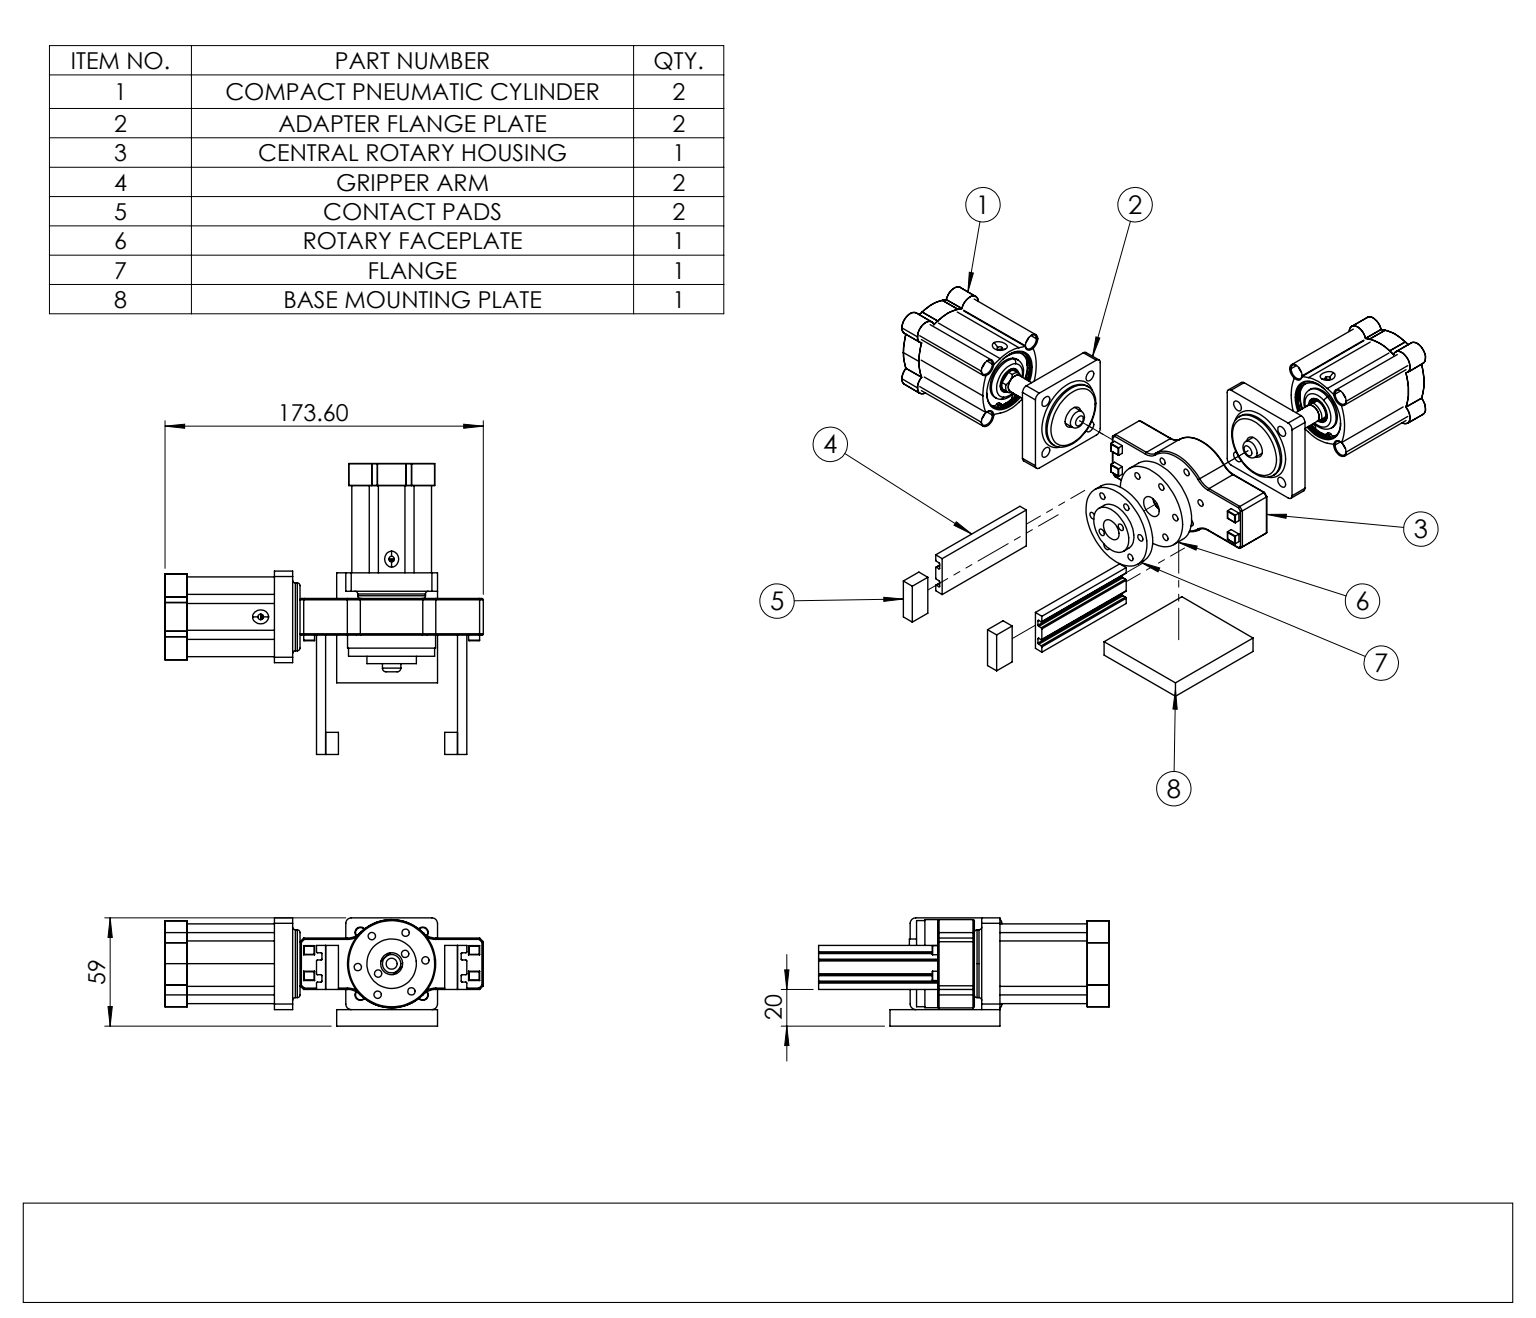
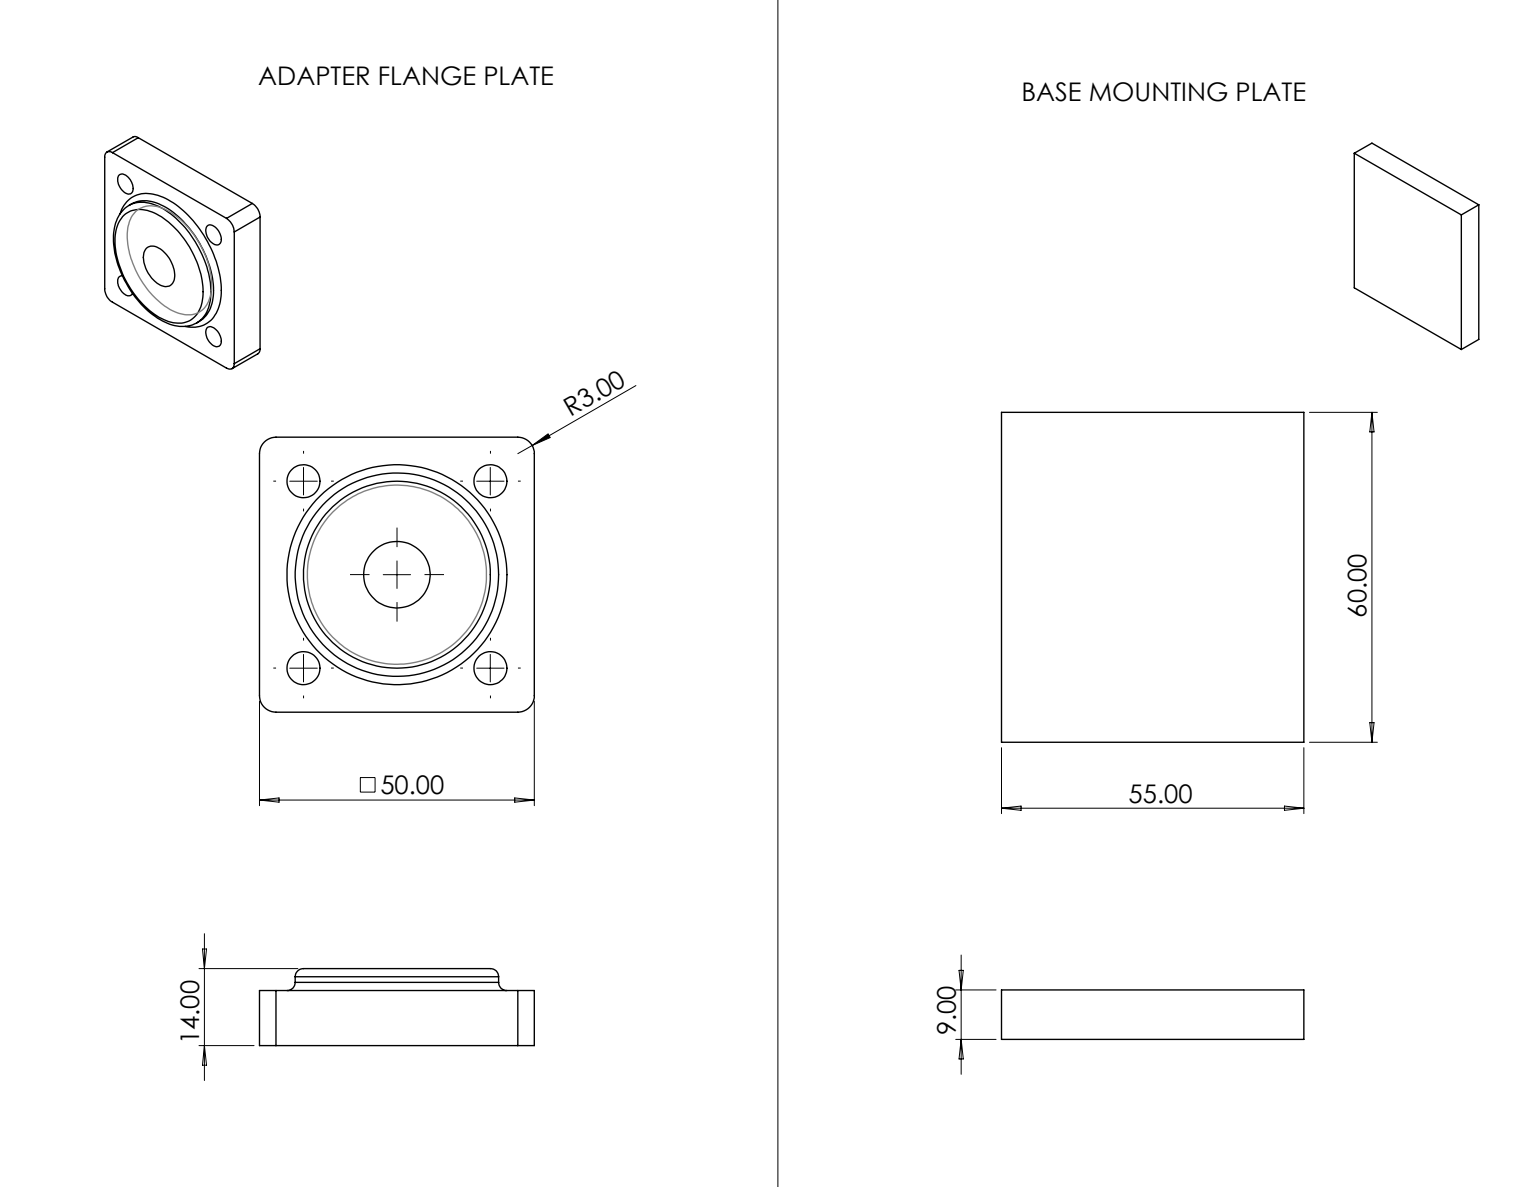
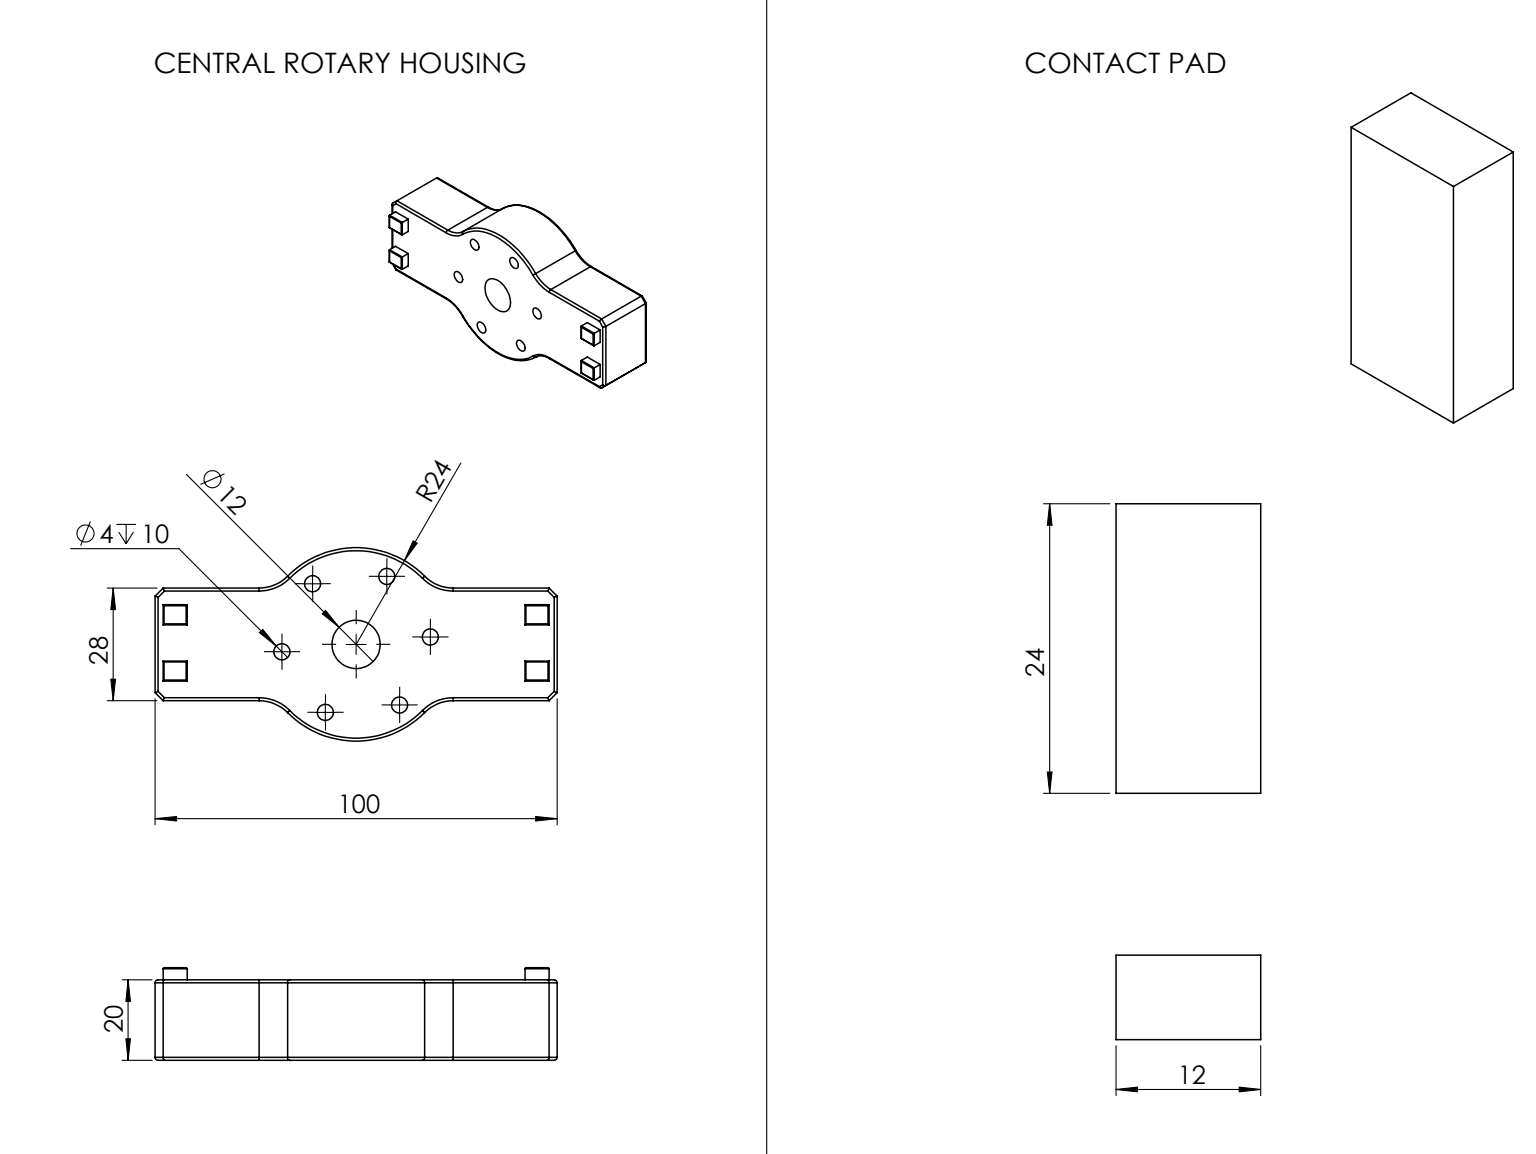
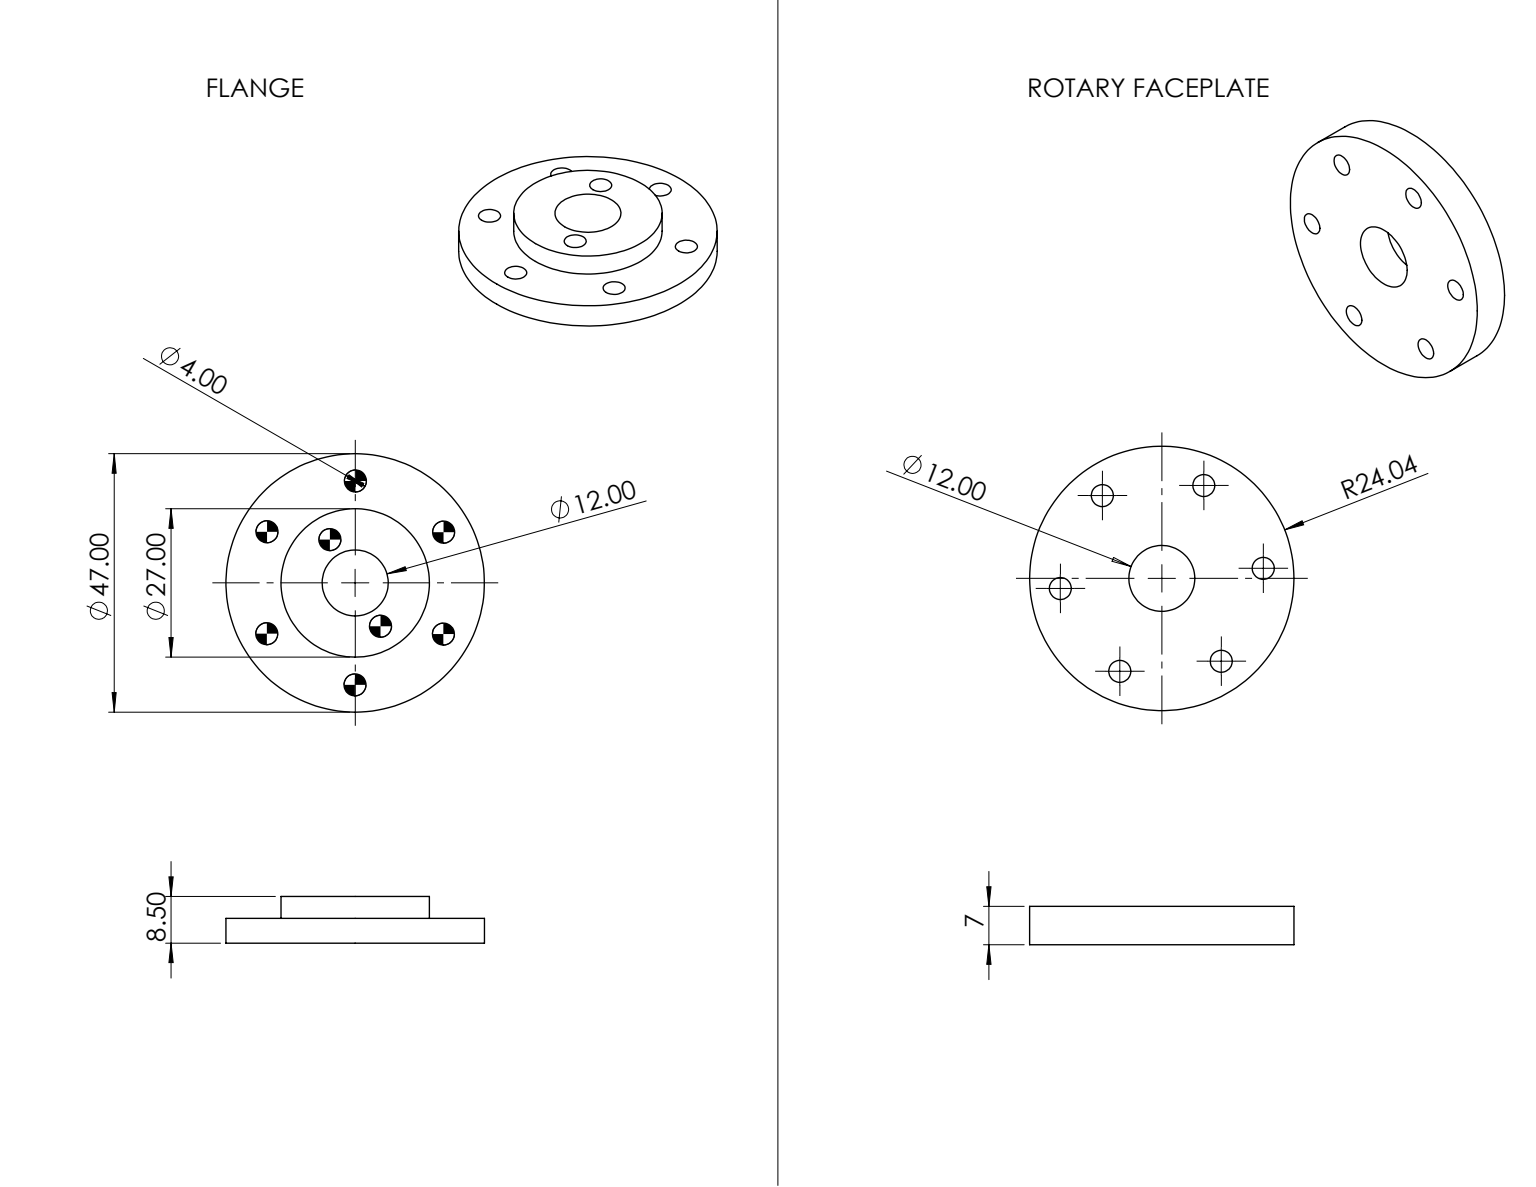
ISO-10303-21;
HEADER;
FILE_DESCRIPTION (('STEP AP214'),
    '1' );
FILE_NAME ('BR-Y-110',
    '2026-10-07T17:53:07',
    ( '' ),
    ( '' ),
    'SwSTEP 2.0',
    'SolidWorks 2025',
    '' );
FILE_SCHEMA (( 'AUTOMOTIVE_DESIGN' ));
ENDSEC;

DATA;
#1 = VERTEX_POINT ( 'NONE', #2797 ) ;
#2 = VERTEX_POINT ( 'NONE', #7279 ) ;
#3 = CARTESIAN_POINT ( 'NONE',  ( -18.05918829504999934, 10.97290950744599947, 5.250000000000000000 ) ) ;
#4 = FACE_OUTER_BOUND ( 'NONE', #8386, .T. ) ;
#5 = LINE ( 'NONE', #10836, #6273 ) ;
#6 = VERTEX_POINT ( 'NONE', #3958 ) ;
#7 = CARTESIAN_POINT ( 'NONE',  ( -0.04028432657539327000, 0.000000000000000000, 20.54539866546728533 ) ) ;
#8 = DIRECTION ( 'NONE',  ( -1.000000000000000000, 0.000000000000000000, 0.000000000000000000 ) ) ;
#9 = VECTOR ( 'NONE', #8104, 1000.000000000000000 ) ;
#10 = AXIS2_PLACEMENT_3D ( 'NONE', #13272, #6842, #503 ) ;
#11 = AXIS2_PLACEMENT_3D ( 'NONE', #8934, #9983, #13191 ) ;
#12 = CARTESIAN_POINT ( 'NONE',  ( -40.33164489498319938, 10.97290950744599947, 5.250000000000000000 ) ) ;
#13 = DIRECTION ( 'NONE',  ( 0.000000000000000000, 0.000000000000000000, 1.000000000000000000 ) ) ;
#14 = EDGE_CURVE ( 'NONE', #8213, #13437, #9334, .T. ) ;
#15 = ORIENTED_EDGE ( 'NONE', *, *, #6104, .F. ) ;
#16 = AXIS2_PLACEMENT_3D ( 'NONE', #5876, #10870, #7634 ) ;
#17 = DIRECTION ( 'NONE',  ( -1.000000000000000000, 0.000000000000000000, 0.000000000000000000 ) ) ;
#18 = VECTOR ( 'NONE', #2959, 1000.000000000000000 ) ;
#19 = CIRCLE ( 'NONE', #13399, 4.000000000000000888 ) ;
#20 = ORIENTED_EDGE ( 'NONE', *, *, #13229, .F. ) ;
#21 = ORIENTED_EDGE ( 'NONE', *, *, #12073, .F. ) ;
#22 = ORIENTED_EDGE ( 'NONE', *, *, #9153, .T. ) ;
#23 = EDGE_LOOP ( 'NONE', ( #6039, #6851, #1913, #2067 ) ) ;
#24 = CARTESIAN_POINT ( 'NONE',  ( -26.35918829505000005, 10.97290950744599947, 61.86500000000000199 ) ) ;
#25 = CARTESIAN_POINT ( 'NONE',  ( 43.38563590245419732, 87.34974178189119698, 20.00000000000000000 ) ) ;
#26 = EDGE_LOOP ( 'NONE', ( #8749, #11948, #13282, #3929 ) ) ;
#27 = DIRECTION ( 'NONE',  ( 0.000000000000000000, 0.000000000000000000, -1.000000000000000000 ) ) ;
#28 = FACE_OUTER_BOUND ( 'NONE', #13183, .T. ) ;
#29 = DIRECTION ( 'NONE',  ( 0.000000000000000000, -1.000000000000000000, 0.000000000000000000 ) ) ;
#30 = CARTESIAN_POINT ( 'NONE',  ( -18.05918829504999934, 10.97290950744599947, 57.35000000000000142 ) ) ;
#31 = DIRECTION ( 'NONE',  ( -0.000000000000000000, 1.000000000000000000, -0.000000000000000000 ) ) ;
#32 = VECTOR ( 'NONE', #959, 1000.000000000000000 ) ;
#33 = CIRCLE ( 'NONE', #3398, 4.749999999999997335 ) ;
#34 = ADVANCED_FACE ( 'NONE', ( #9475 ), #12553, .F. ) ;
#35 = ADVANCED_FACE ( 'NONE', ( #1932 ), #13451, .T. ) ;
#36 = EDGE_CURVE ( 'NONE', #826, #10489, #4183, .T. ) ;
#37 =( GEOMETRIC_REPRESENTATION_CONTEXT ( 3 ) GLOBAL_UNCERTAINTY_ASSIGNED_CONTEXT ( ( #1666 ) ) GLOBAL_UNIT_ASSIGNED_CONTEXT ( ( #5163, #1674, #7109 ) ) REPRESENTATION_CONTEXT ( 'NONE', 'WORKASPACE' ) );
#38 = CARTESIAN_POINT ( 'NONE',  ( 74.18094369249178044, 97.20665973629650125, 10.00000000000000000 ) ) ;
#39 = FACE_BOUND ( 'NONE', #10748, .T. ) ;
#40 = CARTESIAN_POINT ( 'NONE',  ( -23.49332020752115113, 0.2738342970428629952, 62.85000000000000142 ) ) ;
#41 = DIRECTION ( 'NONE',  ( 1.000000000000000000, 0.000000000000000000, 0.000000000000000000 ) ) ;
#42 = CARTESIAN_POINT ( 'NONE',  ( -18.32356812262639068, 30.35913048975403683, 52.99871736656052690 ) ) ;
#43 = DIRECTION ( 'NONE',  ( 0.000000000000000000, 1.000000000000000000, 0.000000000000000000 ) ) ;
#44 = CARTESIAN_POINT ( 'NONE',  ( -18.05918829505001355, 3.709013078446008027, 62.03182374100007479 ) ) ;
#45 = CARTESIAN_POINT ( 'NONE',  ( 68.49370948373500312, 113.0390816101113387, 0.7500000000000006661 ) ) ;
#46 = CARTESIAN_POINT ( 'NONE',  ( -1.904759825251885141, 5.678153534393399759, 62.14999999999999858 ) ) ;
#47 = DIRECTION ( 'NONE',  ( -0.000000000000000000, -0.000000000000000000, -1.000000000000000000 ) ) ;
#48 =( NAMED_UNIT ( * ) SI_UNIT ( $, .STERADIAN. ) SOLID_ANGLE_UNIT ( ) );
#49 = CONICAL_SURFACE ( 'NONE', #4748, 17.00000000000000000, 0.7853981633974476129 ) ;
#50 = EDGE_CURVE ( 'NONE', #1000, #13804, #2021, .T. ) ;
#51 = VERTEX_POINT ( 'NONE', #6255 ) ;
#52 = DIRECTION ( 'NONE',  ( 0.000000000000000000, 0.000000000000000000, 1.000000000000000000 ) ) ;
#53 = ORIENTED_EDGE ( 'NONE', *, *, #11858, .F. ) ;
#54 = VERTEX_POINT ( 'NONE', #10526 ) ;
#55 = CARTESIAN_POINT ( 'NONE',  ( -10.25088531517542023, -8.860076549334110041, 17.25000000000000000 ) ) ;
#56 = CIRCLE ( 'NONE', #12775, 5.000000000000000888 ) ;
#57 = CARTESIAN_POINT ( 'NONE',  ( -18.05918829504999934, 10.97290950744599947, 64.85000000000000853 ) ) ;
#58 = SURFACE_SIDE_STYLE ('',( #2323 ) ) ;
#59 = ORIENTED_EDGE ( 'NONE', *, *, #13776, .F. ) ;
#60 = PLANE ( 'NONE',  #2670 ) ;
#61 = EDGE_CURVE ( 'NONE', #8730, #12568, #7625, .T. ) ;
#62 = DIRECTION ( 'NONE',  ( 1.000000000000000000, 0.000000000000000000, 0.000000000000000000 ) ) ;
#63 = CARTESIAN_POINT ( 'NONE',  ( -5.631644894983189431, 10.97290950744599947, 17.25000000000000000 ) ) ;
#64 = AXIS2_PLACEMENT_3D ( 'NONE', #1240, #10758, #11538 ) ;
#65 = ORIENTED_EDGE ( 'NONE', *, *, #6040, .F. ) ;
#66 = EDGE_CURVE ( 'NONE', #2, #10148, #3731, .T. ) ;
#67 = CARTESIAN_POINT ( 'NONE',  ( 6.940811704950004213, 32.97290950744599769, 10.00000000000000000 ) ) ;
#68 = VERTEX_POINT ( 'NONE', #167 ) ;
#69 = FACE_OUTER_BOUND ( 'NONE', #8366, .T. ) ;
#70 = EDGE_CURVE ( 'NONE', #6919, #7844, #9610, .T. ) ;
#71 = DIRECTION ( 'NONE',  ( -1.000000000000000000, 0.000000000000000000, -0.000000000000000000 ) ) ;
#72 = CARTESIAN_POINT ( 'NONE',  ( 50.63563590245420443, 104.1554980190242361, 22.75000000000000000 ) ) ;
#73 = LINE ( 'NONE', #12845, #11581 ) ;
#74 = DIRECTION ( 'NONE',  ( 0.7071067811865451302, -0.7071067811865500152, 0.000000000000000000 ) ) ;
#75 = EDGE_CURVE ( 'NONE', #10483, #2779, #7556, .T. ) ;
#76 = AXIS2_PLACEMENT_3D ( 'NONE', #7169, #9139, #1729 ) ;
#77 = CARTESIAN_POINT ( 'NONE',  ( -24.37001676333060018, -4.028726038184999858, 62.14999999999999858 ) ) ;
#78 = FACE_OUTER_BOUND ( 'NONE', #2382, .T. ) ;
#79 = EDGE_LOOP ( 'NONE', ( #3659, #11191, #12245, #181 ) ) ;
#80 = EDGE_CURVE ( 'NONE', #9144, #4985, #2152, .T. ) ;
#81 = FACE_OUTER_BOUND ( 'NONE', #12463, .T. ) ;
#82 = ORIENTED_EDGE ( 'NONE', *, *, #9714, .T. ) ;
#83 = ORIENTED_EDGE ( 'NONE', *, *, #1868, .T. ) ;
#84 = EDGE_LOOP ( 'NONE', ( #6155, #12083, #10918, #3272 ) ) ;
#85 = DIRECTION ( 'NONE',  ( 0.000000000000000000, 0.000000000000000000, 1.000000000000000000 ) ) ;
#86 = DIRECTION ( 'NONE',  ( 0.7071067811865525687, 0.7071067811865425767, -0.000000000000000000 ) ) ;
#87 = VERTEX_POINT ( 'NONE', #8553 ) ;
#88 = EDGE_CURVE ( 'NONE', #10198, #10544, #1083, .T. ) ;
#89 = CARTESIAN_POINT ( 'NONE',  ( 142.6356359024541973, 87.03908161011133870, 19.25000000000000000 ) ) ;
#90 = CARTESIAN_POINT ( 'NONE',  ( -19.42965429280413048, 26.91526772932534683, 56.72114474750378577 ) ) ;
#91 = CARTESIAN_POINT ( 'NONE',  ( 7.347880794884120722E-16, 0.000000000000000000, -6.000000000000000888 ) ) ;
#92 = FACE_OUTER_BOUND ( 'NONE', #5027, .T. ) ;
#93 = DIRECTION ( 'NONE',  ( 0.000000000000000000, 0.000000000000000000, -1.000000000000000000 ) ) ;
#94 = ORIENTED_EDGE ( 'NONE', *, *, #9388, .F. ) ;
#95 = VERTEX_POINT ( 'NONE', #8619 ) ;
#96 = CARTESIAN_POINT ( 'NONE',  ( -15.05918829504999756, 10.97290950744599947, 118.8499999999999943 ) ) ;
#97 = ORIENTED_EDGE ( 'NONE', *, *, #11700, .F. ) ;
#98 = DIRECTION ( 'NONE',  ( 0.000000000000000000, 0.000000000000000000, 1.000000000000000000 ) ) ;
#99 = DIRECTION ( 'NONE',  ( 0.000000000000000000, 0.000000000000000000, 1.000000000000000000 ) ) ;
#100 = DIRECTION ( 'NONE',  ( 0.000000000000000000, 0.000000000000000000, -1.000000000000000000 ) ) ;
#101 = AXIS2_PLACEMENT_3D ( 'NONE', #2685, #3784, #6912 ) ;
#102 = CARTESIAN_POINT ( 'NONE',  ( 44.76431555889455183, 85.34974178189114014, 2.983588460272618114E-16 ) ) ;
#103 = CARTESIAN_POINT ( 'NONE',  ( -29.51816008892539855, -2.179141222803619993, 63.45000000000000284 ) ) ;
#104 = ORIENTED_EDGE ( 'NONE', *, *, #12811, .F. ) ;
#105 = CARTESIAN_POINT ( 'NONE',  ( -3.531395436049983960, 3.709013078445997369, 62.03182374100001084 ) ) ;
#106 = CARTESIAN_POINT ( 'NONE',  ( 141.8856359024541973, 87.34974178189115435, 20.00000000000000000 ) ) ;
#107 = CARTESIAN_POINT ( 'NONE',  ( -20.77625425128555392, 5.623371902244430842, 57.35000000000000142 ) ) ;
#108 = CARTESIAN_POINT ( 'NONE',  ( 123.1053058165644671, 129.5087515242213669, 0.7500000000000000000 ) ) ;
#109 =( LENGTH_UNIT ( ) NAMED_UNIT ( * ) SI_UNIT ( .MILLI., .METRE. ) );
#110 = CLOSED_SHELL ( 'NONE', ( #5060, #3881, #6623, #9987, #3732, #7105, #7461, #11688, #1191, #4265, #947, #3436, #2543, #10818, #12397, #3818, #11545, #6558, #4609, #2381, #2843, #3214, #13267, #5308, #5232, #10919, #9049, #5614, #7802, #750 ) ) ;
#111 = EDGE_CURVE ( 'NONE', #2836, #5819, #1718, .T. ) ;
#112 = EDGE_CURVE ( 'NONE', #4329, #209, #6197, .T. ) ;
#113 = AXIS2_PLACEMENT_3D ( 'NONE', #7430, #11720, #2167 ) ;
#114 = DIRECTION ( 'NONE',  ( 0.000000000000000000, 0.000000000000000000, 1.000000000000000000 ) ) ;
#115 = EDGE_LOOP ( 'NONE', ( #6121, #285 ) ) ;
#116 = ORIENTED_EDGE ( 'NONE', *, *, #8831, .F. ) ;
#117 = ORIENTED_EDGE ( 'NONE', *, *, #6877, .T. ) ;
#118 = PLANE ( 'NONE',  #6613 ) ;
#119 = DIRECTION ( 'NONE',  ( 0.000000000000000000, 0.000000000000000000, 1.000000000000000000 ) ) ;
#120 = CARTESIAN_POINT ( 'NONE',  ( 0.000000000000000000, 0.000000000000000000, 0.000000000000000000 ) ) ;
#121 = CYLINDRICAL_SURFACE ( 'NONE', #12455, 6.000000000000000888 ) ;
#122 = LINE ( 'NONE', #4468, #12298 ) ;
#123 = AXIS2_PLACEMENT_3D ( 'NONE', #1081, #954, #12877 ) ;
#124 = DIRECTION ( 'NONE',  ( 0.000000000000000000, 0.000000000000000000, 1.000000000000000000 ) ) ;
#125 = CARTESIAN_POINT ( 'NONE',  ( -18.05918829504999934, 10.97290950744599947, 68.84999999999999432 ) ) ;
#126 = EDGE_CURVE ( 'NONE', #1534, #5295, #6389, .T. ) ;
#127 = UNCERTAINTY_MEASURE_WITH_UNIT (LENGTH_MEASURE( 1.000000000000000082E-05 ), #7321, 'distance_accuracy_value', 'NONE');
#128 = ADVANCED_FACE ( 'NONE', ( #1149 ), #7351, .F. ) ;
#129 = VERTEX_POINT ( 'NONE', #4238 ) ;
#130 = EDGE_CURVE ( 'NONE', #6071, #11290, #13719, .T. ) ;
#131 = CARTESIAN_POINT ( 'NONE',  ( -15.41688231577083101, 30.20956267305470178, 54.20385837980890642 ) ) ;
#132 = SURFACE_STYLE_FILL_AREA ( #10766 ) ;
#133 = DIRECTION ( 'NONE',  ( 0.000000000000000000, 0.000000000000000000, 1.000000000000000000 ) ) ;
#134 = FACE_OUTER_BOUND ( 'NONE', #5191, .T. ) ;
#135 = VERTEX_POINT ( 'NONE', #8486 ) ;
#136 = PLANE ( 'NONE',  #5988 ) ;
#137 = DIRECTION ( 'NONE',  ( -0.000000000000000000, -0.000000000000000000, -1.000000000000000000 ) ) ;
#138 = DIRECTION ( 'NONE',  ( 0.000000000000000000, 0.000000000000000000, 1.000000000000000000 ) ) ;
#139 = ADVANCED_FACE ( 'NONE', ( #10588 ), #13367, .T. ) ;
#140 = VECTOR ( 'NONE', #5917, 1000.000000000000114 ) ;
#141 = DIRECTION ( 'NONE',  ( -0.000000000000000000, -0.000000000000000000, -1.000000000000000000 ) ) ;
#142 = ORIENTED_EDGE ( 'NONE', *, *, #754, .F. ) ;
#143 = EDGE_CURVE ( 'NONE', #7877, #9433, #12710, .T. ) ;
#144 = DIRECTION ( 'NONE',  ( 0.000000000000000000, 0.000000000000000000, -1.000000000000000000 ) ) ;
#145 = ORIENTED_EDGE ( 'NONE', *, *, #6603, .F. ) ;
#146 = ORIENTED_EDGE ( 'NONE', *, *, #5230, .T. ) ;
#147 = VECTOR ( 'NONE', #7020, 1000.000000000000000 ) ;
#148 = CARTESIAN_POINT ( 'NONE',  ( -25.33503448090910126, -7.245613863947209410, 64.85000000000000853 ) ) ;
#149 = LINE ( 'NONE', #12938, #855 ) ;
#150 = ORIENTED_EDGE ( 'NONE', *, *, #10812, .F. ) ;
#151 = CARTESIAN_POINT ( 'NONE',  ( -1.059188295049996231, -6.027090492554000534, 7.250000000000000000 ) ) ;
#152 = CARTESIAN_POINT ( 'NONE',  ( 5.999999999999999112, -12.00000000000000178, 7.000000000000000000 ) ) ;
#153 = LINE ( 'NONE', #1273, #6867 ) ;
#154 = CARTESIAN_POINT ( 'NONE',  ( -30.48673169511680214, 10.97290950744599947, 5.250000000000000000 ) ) ;
#155 = EDGE_CURVE ( 'NONE', #8675, #3193, #8240, .T. ) ;
#156 = FACE_OUTER_BOUND ( 'NONE', #2583, .T. ) ;
#157 = SHAPE_DEFINITION_REPRESENTATION ( #3699, #5502 ) ;
#158 = AXIS2_PLACEMENT_3D ( 'NONE', #4444, #13785, #5467 ) ;
#159 = VERTEX_POINT ( 'NONE', #3135 ) ;
#160 = VECTOR ( 'NONE', #1857, 1000.000000000000000 ) ;
#161 = EDGE_CURVE ( 'NONE', #11468, #4985, #9362, .T. ) ;
#162 = PRODUCT ( 'Contact Pads', 'Contact Pads', '', ( #11558 ) ) ;
#163 = EDGE_LOOP ( 'NONE', ( #919, #320, #6279, #11884 ) ) ;
#164 = EDGE_LOOP ( 'NONE', ( #8775, #9502, #10616, #5660 ) ) ;
#165 = FACE_OUTER_BOUND ( 'NONE', #7206, .T. ) ;
#166 = VECTOR ( 'NONE', #7008, 1000.000000000000000 ) ;
#167 = CARTESIAN_POINT ( 'NONE',  ( -32.05918829504999934, 27.97290950744599769, 10.00000000000000000 ) ) ;
#168 = CIRCLE ( 'NONE', #7293, 6.299999999999998046 ) ;
#169 = CARTESIAN_POINT ( 'NONE',  ( 3.500000000000001776, 2.000000000000000000, 0.000000000000000000 ) ) ;
#170 = AXIS2_PLACEMENT_3D ( 'NONE', #9398, #10575, #4153 ) ;
#171 = CARTESIAN_POINT ( 'NONE',  ( -20.25693731790400776, 30.25607652235614964, 53.78764270006948323 ) ) ;
#172 = VERTEX_POINT ( 'NONE', #11643 ) ;
#173 = CARTESIAN_POINT ( 'NONE',  ( -8.964285665223000521, 0.3335619008453594714, 62.14999999999999858 ) ) ;
#174 = DIRECTION ( 'NONE',  ( 1.000000000000000000, 0.000000000000000000, 0.000000000000000000 ) ) ;
#175 = CARTESIAN_POINT ( 'NONE',  ( -18.05918829504999934, 10.97290950744599947, 67.84999999999999432 ) ) ;
#176 = CARTESIAN_POINT ( 'NONE',  ( -18.05918829504999934, 10.97290950744599947, 56.84999999999999432 ) ) ;
#177 = VECTOR ( 'NONE', #8514, 1000.000000000000000 ) ;
#178 = AXIS2_PLACEMENT_3D ( 'NONE', #8254, #12725, #10295 ) ;
#179 = VECTOR ( 'NONE', #6554, 1000.000000000000000 ) ;
#180 = AXIS2_PLACEMENT_3D ( 'NONE', #7057, #3723, #3934 ) ;
#181 = ORIENTED_EDGE ( 'NONE', *, *, #4608, .T. ) ;
#182 = VERTEX_POINT ( 'NONE', #3404 ) ;
#183 = ORIENTED_EDGE ( 'NONE', *, *, #11008, .T. ) ;
#184 = DIRECTION ( 'NONE',  ( 0.000000000000000000, 0.000000000000000000, 1.000000000000000000 ) ) ;
#185 = ORIENTED_EDGE ( 'NONE', *, *, #5640, .F. ) ;
#186 = ADVANCED_FACE ( 'NONE', ( #7633, #11914, #39, #5265, #12757, #7419 ), #11708, .T. ) ;
#187 = EDGE_LOOP ( 'NONE', ( #9761, #8160, #4704, #9504 ) ) ;
#188 = DIRECTION ( 'NONE',  ( -0.000000000000000000, -0.000000000000000000, 1.000000000000000000 ) ) ;
#189 = VERTEX_POINT ( 'NONE', #4908 ) ;
#190 = FACE_OUTER_BOUND ( 'NONE', #11280, .T. ) ;
#191 = CARTESIAN_POINT ( 'NONE',  ( 0.000000000000000000, 0.000000000000000000, 7.000000000000000000 ) ) ;
#192 = VECTOR ( 'NONE', #12361, 1000.000000000000000 ) ;
#193 = FILL_AREA_STYLE_COLOUR ( '', #3402 ) ;
#194 = VERTEX_POINT ( 'NONE', #10221 ) ;
#195 = VECTOR ( 'NONE', #13133, 1000.000000000000114 ) ;
#196 = CARTESIAN_POINT ( 'NONE',  ( -35.05918829505000645, -6.027090492554000534, 7.250000000000000000 ) ) ;
#197 = DIRECTION ( 'NONE',  ( 0.000000000000000000, 0.000000000000000000, -1.000000000000000000 ) ) ;
#198 = VECTOR ( 'NONE', #6806, 999.9999999999998863 ) ;
#199 = CARTESIAN_POINT ( 'NONE',  ( -1.059188295049996231, 27.97290950744599769, 7.250000000000000000 ) ) ;
#200 = CARTESIAN_POINT ( 'NONE',  ( 62.16596598834396303, 68.56941169600129626, 20.00000000000000000 ) ) ;
#201 = ORIENTED_EDGE ( 'NONE', *, *, #8919, .T. ) ;
#202 = AXIS2_PLACEMENT_3D ( 'NONE', #3684, #7923, #11148 ) ;
#203 = CIRCLE ( 'NONE', #9813, 17.00000000000000355 ) ;
#204 = CARTESIAN_POINT ( 'NONE',  ( -16.07719306376069568, 30.27579076690150117, 53.62366803667482174 ) ) ;
#205 = ADVANCED_FACE ( 'NONE', ( #704 ), #2436, .F. ) ;
#206 = EDGE_CURVE ( 'NONE', #7753, #7831, #10944, .T. ) ;
#207 = ORIENTED_EDGE ( 'NONE', *, *, #1883, .F. ) ;
#208 = DIRECTION ( 'NONE',  ( 0.000000000000000000, 0.000000000000000000, 1.000000000000000000 ) ) ;
#209 = VERTEX_POINT ( 'NONE', #11330 ) ;
#210 = PRESENTATION_STYLE_ASSIGNMENT (( #5374 ) ) ;
#211 = CARTESIAN_POINT ( 'NONE',  ( 42.63563590245419732, 87.03908161011136713, 0.7500000000000006661 ) ) ;
#212 = FACE_OUTER_BOUND ( 'NONE', #7387, .T. ) ;
#213 = CARTESIAN_POINT ( 'NONE',  ( -24.10918829505000005, 10.97290950744599947, 64.85000000000000853 ) ) ;
#214 = AXIS2_PLACEMENT_3D ( 'NONE', #10840, #5509, #2126 ) ;
#215 = AXIS2_PLACEMENT_3D ( 'NONE', #11989, #2447, #13100 ) ;
#216 = ORIENTED_EDGE ( 'NONE', *, *, #2968, .F. ) ;
#217 = VERTEX_POINT ( 'NONE', #6667 ) ;
#218 = ORIENTED_EDGE ( 'NONE', *, *, #1514, .T. ) ;
#219 = DIRECTION ( 'NONE',  ( 0.000000000000000000, 0.000000000000000000, 1.000000000000000000 ) ) ;
#220 = ORIENTED_EDGE ( 'NONE', *, *, #13475, .F. ) ;
#221 = EDGE_CURVE ( 'NONE', #8225, #10962, #1891, .T. ) ;
#222 = ORIENTED_EDGE ( 'NONE', *, *, #6909, .F. ) ;
#223 = VERTEX_POINT ( 'NONE', #1688 ) ;
#224 = VECTOR ( 'NONE', #4940, 1000.000000000000114 ) ;
#225 = PRODUCT_DEFINITION_SHAPE ( 'NONE', 'NONE',  #13814 ) ;
#226 = CIRCLE ( 'NONE', #12506, 15.45000000000000462 ) ;
#227 = CONICAL_SURFACE ( 'NONE', #2931, 8.300000000000000711, 0.08573846772804097349 ) ;
#228 = AXIS2_PLACEMENT_3D ( 'NONE', #13430, #6224, #8258 ) ;
#230 = EDGE_CURVE ( 'NONE', #7248, #13568, #2901, .T. ) ;
#229 = MANIFOLD_SOLID_BREP ( 'Boss-Extrude1', #6124 ) ;
#231 = CYLINDRICAL_SURFACE ( 'NONE', #5745, 0.2500000000000002220 ) ;
#232 = DIRECTION ( 'NONE',  ( 0.000000000000000000, 0.000000000000000000, 1.000000000000000000 ) ) ;
#233 = EDGE_LOOP ( 'NONE', ( #8305, #2316, #6219, #5928, #5645 ) ) ;
#234 = EDGE_CURVE ( 'NONE', #8205, #12910, #5618, .T. ) ;
#235 = FACE_OUTER_BOUND ( 'NONE', #11663, .T. ) ;
#236 = DIRECTION ( 'NONE',  ( -1.000000000000000000, 0.000000000000000000, 0.000000000000000000 ) ) ;
#237 = CARTESIAN_POINT ( 'NONE',  ( -18.05918829504999223, 19.28555359244598932, 63.26601075299999621 ) ) ;
#238 = CARTESIAN_POINT ( 'NONE',  ( -1.059188295049996231, 27.97290950744599769, 68.85549045786049760 ) ) ;
#239 = ADVANCED_FACE ( 'NONE', ( #2830 ), #5929, .T. ) ;
#240 = DIRECTION ( 'NONE',  ( 1.000000000000000000, 0.000000000000000000, 0.000000000000000000 ) ) ;
#241 = CIRCLE ( 'NONE', #3164, 3.450000000000001510 ) ;
#242 = AXIS2_PLACEMENT_3D ( 'NONE', #3348, #13046, #1170 ) ;
#243 = VECTOR ( 'NONE', #2841, 1000.000000000000000 ) ;
#244 = CIRCLE ( 'NONE', #12065, 6.449999999999997513 ) ;
#245 = ORIENTED_EDGE ( 'NONE', *, *, #4667, .T. ) ;
#246 = EDGE_LOOP ( 'NONE', ( #8019, #3663 ) ) ;
#247 = ADVANCED_FACE ( 'NONE', ( #9168 ), #6923, .T. ) ;
#248 = DIRECTION ( 'NONE',  ( 1.000000000000000000, 0.000000000000000000, 0.000000000000000000 ) ) ;
#249 = ORIENTED_EDGE ( 'NONE', *, *, #1249, .F. ) ;
#250 = DIRECTION ( 'NONE',  ( 0.000000000000000000, 0.000000000000000000, -1.000000000000000000 ) ) ;
#251 = EDGE_LOOP ( 'NONE', ( #7690, #10577, #8112, #1921 ) ) ;
#252 = PLANE ( 'NONE',  #16 ) ;
#253 = CARTESIAN_POINT ( 'NONE',  ( 0.000000000000000000, 0.000000000000000000, 7.000000000000000000 ) ) ;
#254 = CARTESIAN_POINT ( 'NONE',  ( -19.60333775920156185, 30.30889438432964056, 53.36507960493299407 ) ) ;
#255 =( GEOMETRIC_REPRESENTATION_CONTEXT ( 3 ) GLOBAL_UNCERTAINTY_ASSIGNED_CONTEXT ( ( #9779 ) ) GLOBAL_UNIT_ASSIGNED_CONTEXT ( ( #8310, #2817, #5089 ) ) REPRESENTATION_CONTEXT ( 'NONE', 'WORKASPACE' ) );
#256 = CIRCLE ( 'NONE', #8054, 7.618085573000000110 ) ;
#257 = CYLINDRICAL_SURFACE ( 'NONE', #13000, 0.5000000000000004441 ) ;
#258 = ORIENTED_EDGE ( 'NONE', *, *, #1830, .F. ) ;
#259 = DIRECTION ( 'NONE',  ( 0.000000000000000000, 0.000000000000000000, 1.000000000000000000 ) ) ;
#260 = VECTOR ( 'NONE', #6397, 1000.000000000000000 ) ;
#261 = DIRECTION ( 'NONE',  ( 1.000000000000000000, 0.000000000000000000, 0.000000000000000000 ) ) ;
#262 = CARTESIAN_POINT ( 'NONE',  ( 140.6356359024541973, 113.0390816101113245, 0.7500000000000000000 ) ) ;
#263 = EDGE_CURVE ( 'NONE', #9409, #2919, #1933, .T. ) ;
#264 = CARTESIAN_POINT ( 'NONE',  ( -3.499999999999998224, 2.499999999999999556, 0.000000000000000000 ) ) ;
#265 = CIRCLE ( 'NONE', #7605, 16.66282263685194920 ) ;
#266 = CIRCLE ( 'NONE', #12968, 3.000000000000002665 ) ;
#267 = ORIENTED_EDGE ( 'NONE', *, *, #6326, .T. ) ;
#268 = CIRCLE ( 'NONE', #8070, 9.999999999999994671 ) ;
#269 = ORIENTED_EDGE ( 'NONE', *, *, #4933, .T. ) ;
#270 = LINE ( 'NONE', #7860, #10180 ) ;
#271 = ORIENTED_EDGE ( 'NONE', *, *, #8365, .T. ) ;
#272 = CARTESIAN_POINT ( 'NONE',  ( -32.35918829505000360, -6.027090492554000534, 58.85000000000000142 ) ) ;
#273 = CARTESIAN_POINT ( 'NONE',  ( -12.26420230435512160, 9.417873376788568507, 67.84999999999999432 ) ) ;
#274 = DIRECTION ( 'NONE',  ( 0.000000000000000000, 1.000000000000000000, 0.000000000000000000 ) ) ;
#275 = FACE_OUTER_BOUND ( 'NONE', #13534, .T. ) ;
#276 = FACE_BOUND ( 'NONE', #615, .T. ) ;
#277 = CARTESIAN_POINT ( 'NONE',  ( -25.33503448090910126, -7.245613863947209410, 7.250000000000000000 ) ) ;
#278 = FACE_OUTER_BOUND ( 'NONE', #4596, .T. ) ;
#279 = EDGE_CURVE ( 'NONE', #9088, #13769, #8829, .T. ) ;
#280 = VECTOR ( 'NONE', #607, 1000.000000000000000 ) ;
#281 = DIRECTION ( 'NONE',  ( -1.000000000000000000, 0.000000000000000000, 0.000000000000000000 ) ) ;
#282 = ADVANCED_FACE ( 'NONE', ( #9827 ), #5462, .T. ) ;
#283 = CARTESIAN_POINT ( 'NONE',  ( 101.4499059006094512, 83.97306027416853169, 10.00000000000000000 ) ) ;
#284 = COLOUR_RGB ( '', 0.66274510, 0.83137255, 0.94901961) ;
#285 = ORIENTED_EDGE ( 'NONE', *, *, #12452, .F. ) ;
#286 = AXIS2_PLACEMENT_3D ( 'NONE', #2851, #528, #4856 ) ;
#287 = ORIENTED_EDGE ( 'NONE', *, *, #11211, .T. ) ;
#288 = CARTESIAN_POINT ( 'NONE',  ( -18.05918829504999934, 30.36027202460864771, 52.99086025162979752 ) ) ;
#289 = SURFACE_SIDE_STYLE ('',( #132 ) ) ;
#290 = CARTESIAN_POINT ( 'NONE',  ( -18.05918829249645086, 2.672909507443099741, 63.15000000009349179 ) ) ;
#291 = CARTESIAN_POINT ( 'NONE',  ( -20.77625425128555392, 5.623371902244430842, 57.35000000000000142 ) ) ;
#292 = LINE ( 'NONE', #13064, #9783 ) ;
#293 = CARTESIAN_POINT ( 'NONE',  ( 3.690811704950004657, 27.97290950744599769, 68.85549045786049760 ) ) ;
#294 = DIRECTION ( 'NONE',  ( 0.000000000000000000, 0.000000000000000000, 1.000000000000000000 ) ) ;
#295 = CIRCLE ( 'NONE', #286, 24.03999999999999915 ) ;
#296 = EDGE_CURVE ( 'NONE', #13765, #13437, #12321, .T. ) ;
#297 = ADVANCED_FACE ( 'NONE', ( #9087, #3790 ), #4208, .F. ) ;
#298 = ORIENTED_EDGE ( 'NONE', *, *, #13475, .T. ) ;
#299 = EDGE_CURVE ( 'NONE', #2876, #6180, #11927, .T. ) ;
#300 = ORIENTED_EDGE ( 'NONE', *, *, #13287, .F. ) ;
#301 = EDGE_LOOP ( 'NONE', ( #4662, #10708, #11788, #11819 ) ) ;
#302 = DIRECTION ( 'NONE',  ( 0.000000000000000000, 0.000000000000000000, 1.000000000000000000 ) ) ;
#303 = EDGE_LOOP ( 'NONE', ( #9142, #9637, #13068, #4588 ) ) ;
#304 = EDGE_LOOP ( 'NONE', ( #3114, #10069, #6854, #8399 ) ) ;
#305 = CIRCLE ( 'NONE', #3211, 2.000000000000001776 ) ;
#306 = ORIENTED_EDGE ( 'NONE', *, *, #4813, .T. ) ;
#307 = ORIENTED_EDGE ( 'NONE', *, *, #8975, .F. ) ;
#308 = DIRECTION ( 'NONE',  ( 0.4528443260392610026, 0.8915896008669278450, 0.000000000000000000 ) ) ;
#309 = DIRECTION ( 'NONE',  ( -1.000000000000000000, -0.000000000000000000, -0.000000000000000000 ) ) ;
#310 = ORIENTED_EDGE ( 'NONE', *, *, #10181, .F. ) ;
#311 = DIRECTION ( 'NONE',  ( 0.000000000000000000, 0.000000000000000000, 1.000000000000000000 ) ) ;
#312 = DIRECTION ( 'NONE',  ( 0.1353548076753729457, 0.000000000000000000, -0.9907971921837297469 ) ) ;
#313 = DIRECTION ( 'NONE',  ( -0.6615960714621569316, 0.7498604124941123938, 0.000000000000000000 ) ) ;
#314 = DIRECTION ( 'NONE',  ( -1.000000000000000000, 0.000000000000000000, 0.000000000000000000 ) ) ;
#315 = EDGE_CURVE ( 'NONE', #6783, #8119, #5237, .T. ) ;
#316 = ORIENTED_EDGE ( 'NONE', *, *, #12153, .T. ) ;
#317 = ORIENTED_EDGE ( 'NONE', *, *, #5380, .F. ) ;
#318 = VERTEX_POINT ( 'NONE', #915 ) ;
#319 = CYLINDRICAL_SURFACE ( 'NONE', #4383, 15.45000000000000462 ) ;
#320 = ORIENTED_EDGE ( 'NONE', *, *, #2823, .T. ) ;
#321 = DIRECTION ( 'NONE',  ( -0.000000000000000000, -0.000000000000000000, 1.000000000000000000 ) ) ;
#322 = VERTEX_POINT ( 'NONE', #8389 ) ;
#323 = LINE ( 'NONE', #455, #3746 ) ;
#324 = CARTESIAN_POINT ( 'NONE',  ( -21.18139722880372489, 30.14955231547764569, 54.83540917236412326 ) ) ;
#325 = ORIENTED_EDGE ( 'NONE', *, *, #2125, .F. ) ;
#326 = CARTESIAN_POINT ( 'NONE',  ( -18.05918829504999934, 2.872909508741170015, 63.35000000000700027 ) ) ;
#327 = LINE ( 'NONE', #1436, #6881 ) ;
#328 = DIRECTION ( 'NONE',  ( 0.000000000000000000, 0.000000000000000000, 1.000000000000000000 ) ) ;
#329 = DIRECTION ( 'NONE',  ( -0.000000000000000000, -0.000000000000000000, -1.000000000000000000 ) ) ;
#330 = ORIENTED_EDGE ( 'NONE', *, *, #13140, .T. ) ;
#331 = EDGE_CURVE ( 'NONE', #12272, #3141, #6992, .T. ) ;
#332 = EDGE_CURVE ( 'NONE', #6971, #4388, #4137, .T. ) ;
#333 = CARTESIAN_POINT ( 'NONE',  ( 4.599650328638321461, 8.500000000000001776, 5.878124499050803919 ) ) ;
#334 = DIRECTION ( 'NONE',  ( 1.000000000000000000, 0.000000000000000000, 0.000000000000000000 ) ) ;
#335 = ORIENTED_EDGE ( 'NONE', *, *, #4099, .T. ) ;
#336 = DIRECTION ( 'NONE',  ( -0.000000000000000000, 1.000000000000000000, -0.000000000000000000 ) ) ;
#337 = ORIENTED_EDGE ( 'NONE', *, *, #13214, .F. ) ;
#338 = CYLINDRICAL_SURFACE ( 'NONE', #13333, 6.000000000000000888 ) ;
#339 = DIRECTION ( 'NONE',  ( -0.000000000000000000, -0.000000000000000000, -1.000000000000000000 ) ) ;
#340 = DIRECTION ( 'NONE',  ( -0.9496839325805417342, 0.3132098788326399541, 0.000000000000000000 ) ) ;
#341 = LINE ( 'NONE', #9058, #8440 ) ;
#342 = CARTESIAN_POINT ( 'NONE',  ( -34.05918829504999934, 10.97290950744599947, 56.84999999999999432 ) ) ;
#343 = CARTESIAN_POINT ( 'NONE',  ( 142.3249757306743675, 110.9104019536709274, 2.976040314969929885E-15 ) ) ;
#344 = DIRECTION ( 'NONE',  ( -0.000000000000000000, 1.000000000000000000, -0.000000000000000000 ) ) ;
#345 = EDGE_CURVE ( 'NONE', #1822, #1130, #8251, .T. ) ;
#346 = VECTOR ( 'NONE', #9572, 1000.000000000000000 ) ;
#347 =( BOUNDED_CURVE ( )  B_SPLINE_CURVE ( 3, ( #7217, #11495, #8211, #7157 ),
 .UNSPECIFIED., .F., .F. ) 
 B_SPLINE_CURVE_WITH_KNOTS ( ( 4, 4 ),
 ( 3.141592653589792672, 4.712388980384689674 ),
 .UNSPECIFIED. ) 
 CURVE ( )  GEOMETRIC_REPRESENTATION_ITEM ( )  RATIONAL_B_SPLINE_CURVE ( ( 1.000000000000000000, 0.8047378541243649375, 0.8047378541243649375, 1.000000000000000000 ) ) 
 REPRESENTATION_ITEM ( '' )  );
#348 = MANIFOLD_SOLID_BREP ( 'Boss-Extrude1', #11944 ) ;
#349 = VERTEX_POINT ( 'NONE', #11530 ) ;
#350 = EDGE_CURVE ( 'NONE', #12769, #6072, #4260, .T. ) ;
#351 = ORIENTED_EDGE ( 'NONE', *, *, #13017, .F. ) ;
#352 = DIRECTION ( 'NONE',  ( -0.000000000000000000, -0.000000000000000000, -1.000000000000000000 ) ) ;
#353 = ORIENTED_EDGE ( 'NONE', *, *, #4353, .F. ) ;
#354 = CYLINDRICAL_SURFACE ( 'NONE', #1490, 6.049999999999999822 ) ;
#355 = VECTOR ( 'NONE', #352, 1000.000000000000000 ) ;
#356 = DIRECTION ( 'NONE',  ( 1.000000000000000000, 0.000000000000000000, 0.000000000000000000 ) ) ;
#357 = CARTESIAN_POINT ( 'NONE',  ( 50.63563590245420443, 89.90549801902423610, 23.00000000000000000 ) ) ;
#358 = DIRECTION ( 'NONE',  ( 0.000000000000000000, 0.000000000000000000, -1.000000000000000000 ) ) ;
#359 = CYLINDRICAL_SURFACE ( 'NONE', #10271, 1.999999999999995781 ) ;
#360 = FACE_OUTER_BOUND ( 'NONE', #13071, .T. ) ;
#361 = AXIS2_PLACEMENT_3D ( 'NONE', #9633, #52, #5763 ) ;
#362 = ORIENTED_EDGE ( 'NONE', *, *, #6475, .T. ) ;
#363 = VERTEX_POINT ( 'NONE', #5176 ) ;
#364 = DIRECTION ( 'NONE',  ( 1.000000000000000000, 0.000000000000000000, 0.000000000000000000 ) ) ;
#365 = ORIENTED_EDGE ( 'NONE', *, *, #11013, .F. ) ;
#366 = ORIENTED_EDGE ( 'NONE', *, *, #1120, .F. ) ;
#367 = ORIENTED_EDGE ( 'NONE', *, *, #7268, .F. ) ;
#368 = CARTESIAN_POINT ( 'NONE',  ( -32.58698115404997253, 18.23680593644601089, 62.03182374100001084 ) ) ;
#369 = EDGE_CURVE ( 'NONE', #9649, #5856, #6141, .T. ) ;
#370 = CARTESIAN_POINT ( 'NONE',  ( -11.06274345774342116, 24.74796884084004844, 60.65000000000000568 ) ) ;
#371 = ORIENTED_EDGE ( 'NONE', *, *, #6030, .T. ) ;
#372 = CIRCLE ( 'NONE', #1703, 1.725000000000000755 ) ;
#373 = CARTESIAN_POINT ( 'NONE',  ( -17.25681213616876164, 26.95277304015176512, 56.08231620102305470 ) ) ;
#374 = DIRECTION ( 'NONE',  ( 1.000000000000000000, 0.000000000000000000, 0.000000000000000000 ) ) ;
#375 = FACE_OUTER_BOUND ( 'NONE', #11590, .T. ) ;
#376 = EDGE_LOOP ( 'NONE', ( #13002, #6845, #9254, #779 ) ) ;
#377 = ORIENTED_EDGE ( 'NONE', *, *, #5510, .F. ) ;
#378 = LINE ( 'NONE', #13236, #10194 ) ;
#379 = ORIENTED_EDGE ( 'NONE', *, *, #12753, .T. ) ;
#380 = VERTEX_POINT ( 'NONE', #1045 ) ;
#381 = EDGE_CURVE ( 'NONE', #10270, #2929, #13691, .T. ) ;
#382 = LINE ( 'NONE', #4652, #10884 ) ;
#383 = CARTESIAN_POINT ( 'NONE',  ( -21.60736175305857998, 30.08769857173765416, 55.71792893088887411 ) ) ;
#384 = DIRECTION ( 'NONE',  ( 0.000000000000000000, 0.000000000000000000, 1.000000000000000000 ) ) ;
#385 = DIRECTION ( 'NONE',  ( -1.000000000000000000, 0.000000000000000000, 0.000000000000000000 ) ) ;
#386 = DIRECTION ( 'NONE',  ( -0.9496839325805417342, -0.3132098788326399541, 0.000000000000000000 ) ) ;
#387 = LINE ( 'NONE', #8914, #11403 ) ;
#388 = AXIS2_PLACEMENT_3D ( 'NONE', #10817, #5485, #2106 ) ;
#389 = CARTESIAN_POINT ( 'NONE',  ( 116.7775623211734342, 123.0390816101113245, 20.00000000000000000 ) ) ;
#390 = DIRECTION ( 'NONE',  ( 0.000000000000000000, 0.000000000000000000, 1.000000000000000000 ) ) ;
#391 = ORIENTED_EDGE ( 'NONE', *, *, #1074, .T. ) ;
#392 = ORIENTED_EDGE ( 'NONE', *, *, #10970, .T. ) ;
#393 = CIRCLE ( 'NONE', #6637, 4.749999999999997335 ) ;
#394 = AXIS2_PLACEMENT_3D ( 'NONE', #13518, #1937, #13587 ) ;
#395 = EDGE_LOOP ( 'NONE', ( #2584, #2957, #7382, #3323 ) ) ;
#396 = DIRECTION ( 'NONE',  ( 0.000000000000000000, 0.000000000000000000, 1.000000000000000000 ) ) ;
#397 = CYLINDRICAL_SURFACE ( 'NONE', #11158, 6.450000000000009948 ) ;
#398 = ORIENTED_EDGE ( 'NONE', *, *, #7843, .T. ) ;
#399 = CARTESIAN_POINT ( 'NONE',  ( 4.599650328638321461, 8.500000000000000000, 7.878124499050794149 ) ) ;
#400 = EDGE_CURVE ( 'NONE', #2628, #8206, #6299, .T. ) ;
#401 = LINE ( 'NONE', #12069, #13543 ) ;
#402 = FACE_OUTER_BOUND ( 'NONE', #1652, .T. ) ;
#403 = DIRECTION ( 'NONE',  ( 0.000000000000000000, 1.000000000000000000, 0.000000000000000000 ) ) ;
#404 = DIRECTION ( 'NONE',  ( 1.000000000000000000, -0.000000000000000000, 0.000000000000000000 ) ) ;
#405 = LINE ( 'NONE', #3904, #7107 ) ;
#406 = ADVANCED_FACE ( 'NONE', ( #4 ), #7444, .T. ) ;
#407 = LINE ( 'NONE', #1517, #3985 ) ;
#408 = DIRECTION ( 'NONE',  ( -1.239088197126292296E-16, 1.000000000000000000, 0.000000000000000000 ) ) ;
#409 = PLANE ( 'NONE',  #6769 ) ;
#410 = LINE ( 'NONE', #10063, #2675 ) ;
#411 = AXIS2_PLACEMENT_3D ( 'NONE', #10209, #2683, #4898 ) ;
#412 = CIRCLE ( 'NONE', #8208, 24.04163056034261459 ) ;
#413 = CIRCLE ( 'NONE', #2654, 1.999999999999994893 ) ;
#414 = EDGE_CURVE ( 'NONE', #159, #13667, #776, .T. ) ;
#415 = ORIENTED_EDGE ( 'NONE', *, *, #1664, .T. ) ;
#416 = LINE ( 'NONE', #7878, #12614 ) ;
#417 = CIRCLE ( 'NONE', #4437, 1.499999999999999556 ) ;
#418 = VECTOR ( 'NONE', #5319, 1000.000000000000000 ) ;
#419 = AXIS2_PLACEMENT_3D ( 'NONE', #7166, #4046, #8361 ) ;
#420 = ORIENTED_EDGE ( 'NONE', *, *, #7245, .F. ) ;
#421 = ADVANCED_FACE ( 'NONE', ( #4551 ), #12019, .T. ) ;
#422 = DIRECTION ( 'NONE',  ( 0.000000000000000000, 0.000000000000000000, -1.000000000000000000 ) ) ;
#423 = AXIS2_PLACEMENT_3D ( 'NONE', #11901, #6648, #2493 ) ;
#424 = SURFACE_SIDE_STYLE ('',( #6838 ) ) ;
#425 = ORIENTED_EDGE ( 'NONE', *, *, #4953, .T. ) ;
#426 = CARTESIAN_POINT ( 'NONE',  ( -7.499999999999996447, -0.5000000000000019984, 0.000000000000000000 ) ) ;
#427 = PLANE ( 'NONE',  #8021 ) ;
#428 = EDGE_CURVE ( 'NONE', #7051, #87, #10065, .T. ) ;
#429 = CARTESIAN_POINT ( 'NONE',  ( -24.10918829505000005, 10.97290950744599947, 64.85000000000000853 ) ) ;
#430 = CIRCLE ( 'NONE', #8236, 6.145833333000000565 ) ;
#431 = ORIENTED_EDGE ( 'NONE', *, *, #1519, .T. ) ;
#432 = EDGE_LOOP ( 'NONE', ( #10471, #3421, #1762, #3978 ) ) ;
#433 = ORIENTED_EDGE ( 'NONE', *, *, #4646, .T. ) ;
#434 = CARTESIAN_POINT ( 'NONE',  ( -27.49999999999998934, 0.000000000000000000, -30.00000000000000355 ) ) ;
#435 = ORIENTED_EDGE ( 'NONE', *, *, #8093, .T. ) ;
#436 = ORIENTED_EDGE ( 'NONE', *, *, #2415, .T. ) ;
#437 = ORIENTED_EDGE ( 'NONE', *, *, #13232, .F. ) ;
#438 = CARTESIAN_POINT ( 'NONE',  ( 44.63563590245420443, 108.9054980190242503, 23.00000000000000000 ) ) ;
#439 = ORIENTED_EDGE ( 'NONE', *, *, #6372, .F. ) ;
#440 = DIRECTION ( 'NONE',  ( -0.000000000000000000, 1.000000000000000000, -0.000000000000000000 ) ) ;
#441 = ORIENTED_EDGE ( 'NONE', *, *, #8899, .T. ) ;
#442 = CARTESIAN_POINT ( 'NONE',  ( 10.81426999815522549, -15.06602133594279991, -3.000000000000000000 ) ) ;
#443 = CONICAL_SURFACE ( 'NONE', #7785, 16.95000000000000284, 0.7853981633974433940 ) ;
#444 = FACE_OUTER_BOUND ( 'NONE', #7372, .T. ) ;
#445 = AXIS2_PLACEMENT_3D ( 'NONE', #10538, #7564, #4179 ) ;
#446 = DIRECTION ( 'NONE',  ( -1.000000000000000000, 0.000000000000000000, 0.000000000000000000 ) ) ;
#447 = EDGE_CURVE ( 'NONE', #9970, #6077, #6564, .T. ) ;
#448 = CARTESIAN_POINT ( 'NONE',  ( 102.2760581142613603, 115.9375248198690826, 20.00000000000000000 ) ) ;
#449 = ORIENTED_EDGE ( 'NONE', *, *, #12076, .T. ) ;
#450 = VECTOR ( 'NONE', #8530, 1000.000000000000227 ) ;
#451 = VECTOR ( 'NONE', #9676, 1000.000000000000000 ) ;
#452 = ORIENTED_EDGE ( 'NONE', *, *, #263, .F. ) ;
#453 = CARTESIAN_POINT ( 'NONE',  ( 44.88563590245420443, 108.6554980190242503, 23.00000000000000000 ) ) ;
#454 = ORIENTED_EDGE ( 'NONE', *, *, #13612, .T. ) ;
#455 = CARTESIAN_POINT ( 'NONE',  ( 134.6356359024541973, 103.9054980190242361, 20.00000000000000000 ) ) ;
#456 = CARTESIAN_POINT ( 'NONE',  ( -21.14708333414588637, 30.15419697583712733, 54.78115759698135889 ) ) ;
#457 = CARTESIAN_POINT ( 'NONE',  ( -18.05918829504999934, 10.97290950744599947, 57.35000000000000142 ) ) ;
#458 = CARTESIAN_POINT ( 'NONE',  ( -41.50918829505000218, -6.027090492554000534, 17.25000000000000000 ) ) ;
#459 = CARTESIAN_POINT ( 'NONE',  ( -4.599650328638321461, 8.500000000000001776, -7.878124499050794149 ) ) ;
#460 = DIRECTION ( 'NONE',  ( 0.000000000000000000, 0.000000000000000000, -1.000000000000000000 ) ) ;
#461 = DIRECTION ( 'NONE',  ( -0.000000000000000000, -0.000000000000000000, 1.000000000000000000 ) ) ;
#462 = VECTOR ( 'NONE', #11230, 1000.000000000000227 ) ;
#463 = PRODUCT ( 'Adapter Flange Plate', 'Adapter Flange Plate', '', ( #9677 ) ) ;
#464 =( GEOMETRIC_REPRESENTATION_CONTEXT ( 3 ) GLOBAL_UNCERTAINTY_ASSIGNED_CONTEXT ( ( #127 ) ) GLOBAL_UNIT_ASSIGNED_CONTEXT ( ( #7321, #10560, #2120 ) ) REPRESENTATION_CONTEXT ( 'NONE', 'WORKASPACE' ) );
#465 = ADVANCED_FACE ( 'NONE', ( #5437 ), #9788, .T. ) ;
#466 = AXIS2_PLACEMENT_3D ( 'NONE', #5182, #8642, #10822 ) ;
#467 = VERTEX_POINT ( 'NONE', #290 ) ;
#468 = EDGE_CURVE ( 'NONE', #5173, #11089, #3806, .T. ) ;
#469 = EDGE_CURVE ( 'NONE', #3141, #10024, #8658, .T. ) ;
#470 = AXIS2_PLACEMENT_3D ( 'NONE', #9417, #10656, #8354 ) ;
#471 = CARTESIAN_POINT ( 'NONE',  ( -12.54628844161313950, -7.366404416634599883, 63.45000000000000284 ) ) ;
#472 = CONICAL_SURFACE ( 'NONE', #3607, 6.049999999999999822, 0.1357715569457985105 ) ;
#473 =( REPRESENTATION_RELATIONSHIP ('NONE','NONE', #11848, #2236 ) REPRESENTATION_RELATIONSHIP_WITH_TRANSFORMATION ( #12679 )SHAPE_REPRESENTATION_RELATIONSHIP( ) );
#474 = DIRECTION ( 'NONE',  ( 1.000000000000000000, 0.000000000000000000, 0.000000000000000000 ) ) ;
#475 = AXIS2_PLACEMENT_3D ( 'NONE', #3143, #10327, #12625 ) ;
#476 = EDGE_LOOP ( 'NONE', ( #7429, #4886, #7264, #4257 ) ) ;
#477 = CYLINDRICAL_SURFACE ( 'NONE', #9605, 8.299999999999998934 ) ;
#478 = CARTESIAN_POINT ( 'NONE',  ( 44.94629607423406270, 112.2890816101113387, 20.00000000000000000 ) ) ;
#479 = CARTESIAN_POINT ( 'NONE',  ( 0.000000000000000000, -17.50000000000000000, 0.000000000000000000 ) ) ;
#480 = CARTESIAN_POINT ( 'NONE',  ( 0.09777679598749920709, -1.420146627243660031, 68.85549045786049760 ) ) ;
#481 = FACE_BOUND ( 'NONE', #4546, .T. ) ;
#482 = DIRECTION ( 'NONE',  ( -1.000000000000000000, 0.000000000000000000, 0.000000000000000000 ) ) ;
#483 = DIRECTION ( 'NONE',  ( -0.000000000000000000, -0.000000000000000000, 1.000000000000000000 ) ) ;
#484 = DIRECTION ( 'NONE',  ( -0.3132098788326420635, -0.9496839325805410681, 0.000000000000000000 ) ) ;
#485 = DIRECTION ( 'NONE',  ( 0.000000000000000000, 0.000000000000000000, -1.000000000000000000 ) ) ;
#486 =( GEOMETRIC_REPRESENTATION_CONTEXT ( 3 ) GLOBAL_UNCERTAINTY_ASSIGNED_CONTEXT ( ( #1243 ) ) GLOBAL_UNIT_ASSIGNED_CONTEXT ( ( #3583, #2756, #11179 ) ) REPRESENTATION_CONTEXT ( 'NONE', 'WORKASPACE' ) );
#487 = CIRCLE ( 'NONE', #12751, 2.999999999999998224 ) ;
#488 = TOROIDAL_SURFACE ( 'NONE', #8290, 20.00000000000000000, 1.500000000000000000 ) ;
#489 = EDGE_CURVE ( 'NONE', #2763, #3609, #10908, .T. ) ;
#490 = EDGE_CURVE ( 'NONE', #10813, #8384, #10834, .T. ) ;
#491 = ORIENTED_EDGE ( 'NONE', *, *, #6716, .F. ) ;
#492 = ADVANCED_FACE ( 'NONE', ( #5580 ), #11804, .F. ) ;
#493 = CARTESIAN_POINT ( 'NONE',  ( -23.85417428574490373, 12.52794563810342154, 67.84999999999999432 ) ) ;
#494 = ORIENTED_EDGE ( 'NONE', *, *, #12786, .T. ) ;
#495 = EDGE_LOOP ( 'NONE', ( #8465, #5386, #11204, #2294 ) ) ;
#496 = DIRECTION ( 'NONE',  ( 1.000000000000000000, 0.000000000000000000, 0.000000000000000000 ) ) ;
#497 = EDGE_CURVE ( 'NONE', #7929, #3451, #2337, .T. ) ;
#498 = CYLINDRICAL_SURFACE ( 'NONE', #6914, 3.000000000000000000 ) ;
#499 = FILL_AREA_STYLE_COLOUR ( '', #7596 ) ;
#500 = LINE ( 'NONE', #3780, #1311 ) ;
#501 = CARTESIAN_POINT ( 'NONE',  ( 1.640811704950005057, 27.97290950744599769, 7.250000000000000000 ) ) ;
#502 = CARTESIAN_POINT ( 'NONE',  ( -11.75918829505000041, 10.97290950744599947, 61.86500000000000199 ) ) ;
#503 = DIRECTION ( 'NONE',  ( -1.000000000000000000, 0.000000000000000000, 0.000000000000000000 ) ) ;
#504 = EDGE_CURVE ( 'NONE', #3446, #7761, #4041, .T. ) ;
#505 = CIRCLE ( 'NONE', #3415, 0.7500000000000000000 ) ;
#506 = VERTEX_POINT ( 'NONE', #8735 ) ;
#507 = EDGE_CURVE ( 'NONE', #12691, #7299, #11644, .T. ) ;
#508 = CARTESIAN_POINT ( 'NONE',  ( -16.54062941099373063, 30.31058478656570188, 61.34775567103718430 ) ) ;
#509 = ORIENTED_EDGE ( 'NONE', *, *, #7168, .F. ) ;
#510 = VERTEX_POINT ( 'NONE', #1250 ) ;
#511 = EDGE_CURVE ( 'NONE', #2084, #11003, #5649, .T. ) ;
#512 = EDGE_LOOP ( 'NONE', ( #3363, #9806, #10726, #5357 ) ) ;
#513 = FACE_BOUND ( 'NONE', #6731, .T. ) ;
#514 = CARTESIAN_POINT ( 'NONE',  ( 116.7775623211734342, 85.78908161011133870, 0.000000000000000000 ) ) ;
#515 = CARTESIAN_POINT ( 'NONE',  ( -18.05918829504999934, 10.97290950744599947, 61.65955166399999854 ) ) ;
#516 = DIRECTION ( 'NONE',  ( 0.000000000000000000, 0.000000000000000000, 1.000000000000000000 ) ) ;
#517 = AXIS2_PLACEMENT_3D ( 'NONE', #13650, #944, #11756 ) ;
#518 = CYLINDRICAL_SURFACE ( 'NONE', #11011, 6.299999999999999822 ) ;
#519 = CARTESIAN_POINT ( 'NONE',  ( -6.000000000000000888, -12.00000000000000178, 0.000000000000000000 ) ) ;
#520 = CARTESIAN_POINT ( 'NONE',  ( -30.80918829504999934, -6.027090492554000534, 64.35000000000000853 ) ) ;
#521 = ADVANCED_FACE ( 'NONE', ( #9868 ), #13062, .F. ) ;
#522 = ORIENTED_EDGE ( 'NONE', *, *, #7912, .T. ) ;
#523 = EDGE_CURVE ( 'NONE', #7555, #10214, #3846, .T. ) ;
#524 = LINE ( 'NONE', #7913, #11304 ) ;
#525 = VERTEX_POINT ( 'NONE', #6502 ) ;
#526 = CARTESIAN_POINT ( 'NONE',  ( -25.64433075620760150, -3.961216307075045240, 61.85000000000000142 ) ) ;
#527 = CARTESIAN_POINT ( 'NONE',  ( -21.02695553212586432, 30.16999431196798298, 60.09573059200643286 ) ) ;
#528 = DIRECTION ( 'NONE',  ( 0.000000000000000000, 0.000000000000000000, 1.000000000000000000 ) ) ;
#529 = DIRECTION ( 'NONE',  ( 0.000000000000000000, 0.000000000000000000, -1.000000000000000000 ) ) ;
#530 = LINE ( 'NONE', #5893, #7154 ) ;
#531 = AXIS2_PLACEMENT_3D ( 'NONE', #7726, #6695, #2740 ) ;
#532 = DIRECTION ( 'NONE',  ( 0.000000000000000000, 0.000000000000000000, -1.000000000000000000 ) ) ;
#533 = VERTEX_POINT ( 'NONE', #10767 ) ;
#534 = CARTESIAN_POINT ( 'NONE',  ( -18.05918829504999934, 10.00028003023991907, 62.14999999999999858 ) ) ;
#535 = DIRECTION ( 'NONE',  ( 1.000000000000000000, 0.000000000000000000, 0.000000000000000000 ) ) ;
#536 = ORIENTED_EDGE ( 'NONE', *, *, #8265, .F. ) ;
#537 = DIRECTION ( 'NONE',  ( 1.000000000000000000, 0.000000000000000000, 0.000000000000000000 ) ) ;
#538 =( LENGTH_UNIT ( ) NAMED_UNIT ( * ) SI_UNIT ( .MILLI., .METRE. ) );
#539 = FACE_OUTER_BOUND ( 'NONE', #11404, .T. ) ;
#540 = DIRECTION ( 'NONE',  ( 1.000000000000000000, 0.000000000000000000, 0.000000000000000000 ) ) ;
#541 = DIRECTION ( 'NONE',  ( -0.000000000000000000, -1.000000000000000000, -0.000000000000000000 ) ) ;
#542 = DIRECTION ( 'NONE',  ( 0.000000000000000000, 0.000000000000000000, 1.000000000000000000 ) ) ;
#543 = CARTESIAN_POINT ( 'NONE',  ( 134.6356359024541973, 108.9054980190242503, 22.75000000000000000 ) ) ;
#544 = EDGE_CURVE ( 'NONE', #2553, #8162, #1184, .T. ) ;
#545 = DIRECTION ( 'NONE',  ( 1.000000000000000000, 0.000000000000000000, 0.000000000000000000 ) ) ;
#546 = MECHANICAL_DESIGN_GEOMETRIC_PRESENTATION_REPRESENTATION (  '', ( #12596 ), #10109 ) ;
#547 = DIRECTION ( 'NONE',  ( 0.000000000000000000, 0.000000000000000000, -1.000000000000000000 ) ) ;
#548 = DIRECTION ( 'NONE',  ( 0.000000000000000000, 0.000000000000000000, -1.000000000000000000 ) ) ;
#549 = ORIENTED_EDGE ( 'NONE', *, *, #8020, .F. ) ;
#550 = ORIENTED_EDGE ( 'NONE', *, *, #345, .F. ) ;
#551 = CARTESIAN_POINT ( 'NONE',  ( -36.55918829504999934, 10.97290950744599947, 11.50000000000000000 ) ) ;
#552 = ORIENTED_EDGE ( 'NONE', *, *, #7488, .T. ) ;
#553 = ORIENTED_EDGE ( 'NONE', *, *, #616, .F. ) ;
#554 = FACE_OUTER_BOUND ( 'NONE', #6549, .T. ) ;
#555 = FACE_BOUND ( 'NONE', #11070, .T. ) ;
#556 = SURFACE_STYLE_USAGE ( .BOTH. , #424 ) ;
#557 = EDGE_LOOP ( 'NONE', ( #13661, #2052 ) ) ;
#558 = DIRECTION ( 'NONE',  ( 0.000000000000000000, 0.000000000000000000, -1.000000000000000000 ) ) ;
#559 = EDGE_CURVE ( 'NONE', #9088, #7612, #6024, .T. ) ;
#560 = VECTOR ( 'NONE', #10996, 1000.000000000000227 ) ;
#561 = DIRECTION ( 'NONE',  ( -0.7050191076322684935, -0.7091883091770476710, 0.000000000000000000 ) ) ;
#562 = EDGE_CURVE ( 'NONE', #8669, #10489, #2680, .T. ) ;
#563 = CARTESIAN_POINT ( 'NONE',  ( -18.05918829504999934, 10.97290950744599947, 62.14999999999999858 ) ) ;
#564 = DIRECTION ( 'NONE',  ( 0.000000000000000000, 0.000000000000000000, -1.000000000000000000 ) ) ;
#565 = CLOSED_SHELL ( 'NONE', ( #6640, #3677, #5018, #11103, #4713, #11376, #9347, #11175, #12290, #2468, #10794, #12497, #7213, #4834, #4033, #591, #10301, #3376, #8262, #6490, #6495, #4028, #2671, #2050, #11073 ) ) ;
#566 = PRODUCT_DEFINITION ( 'UNKNOWN', '', #9121, #4050 ) ;
#567 = ORIENTED_EDGE ( 'NONE', *, *, #3893, .T. ) ;
#568 = VECTOR ( 'NONE', #12571, 1000.000000000000000 ) ;
#569 = ORIENTED_EDGE ( 'NONE', *, *, #3319, .T. ) ;
#570 = CARTESIAN_POINT ( 'NONE',  ( 83.82136590429891498, 114.1051029460540605, 10.00000000000000000 ) ) ;
#571 = ORIENTED_EDGE ( 'NONE', *, *, #161, .T. ) ;
#572 = DIRECTION ( 'NONE',  ( -1.000000000000000000, 0.000000000000000000, 0.000000000000000000 ) ) ;
#573 = EDGE_LOOP ( 'NONE', ( #4000, #4344 ) ) ;
#574 = FACE_BOUND ( 'NONE', #8182, .T. ) ;
#575 = CARTESIAN_POINT ( 'NONE',  ( -32.58698115404997253, 3.709013078445997369, 62.03182374100001084 ) ) ;
#576 = CARTESIAN_POINT ( 'NONE',  ( -36.21615338608749823, -1.420146627243662030, 64.85000000000000853 ) ) ;
#577 = EDGE_CURVE ( 'NONE', #1997, #8730, #12223, .T. ) ;
#578 = LINE ( 'NONE', #5112, #2725 ) ;
#579 = CARTESIAN_POINT ( 'NONE',  ( -24.37001676333060018, -4.028726038184999858, 62.14999999999999858 ) ) ;
#580 = ORIENTED_EDGE ( 'NONE', *, *, #4518, .F. ) ;
#581 = DIRECTION ( 'NONE',  ( 0.000000000000000000, 0.000000000000000000, 1.000000000000000000 ) ) ;
#582 = AXIS2_PLACEMENT_3D ( 'NONE', #4592, #10119, #13246 ) ;
#583 = CARTESIAN_POINT ( 'NONE',  ( 134.6356359024541973, 94.90549801902425031, 22.75000000000000000 ) ) ;
#584 = EDGE_CURVE ( 'NONE', #1164, #10151, #226, .T. ) ;
#585 = ORIENTED_EDGE ( 'NONE', *, *, #2198, .T. ) ;
#586 = VERTEX_POINT ( 'NONE', #11046 ) ;
#587 = AXIS2_PLACEMENT_3D ( 'NONE', #4402, #8584, #10906 ) ;
#588 = DIRECTION ( 'NONE',  ( 1.000000000000000000, 0.000000000000000000, 0.000000000000000000 ) ) ;
#589 = ORIENTED_EDGE ( 'NONE', *, *, #8356, .F. ) ;
#590 = CARTESIAN_POINT ( 'NONE',  ( -18.05918829504999934, 10.97290950744599947, 63.64999999999999858 ) ) ;
#591 = ADVANCED_FACE ( 'NONE', ( #11178, #689, #555, #1466 ), #9995, .T. ) ;
#592 = CARTESIAN_POINT ( 'NONE',  ( -20.85553867603828593, 30.19135017469169924, 60.31826595084313425 ) ) ;
#593 = DIRECTION ( 'NONE',  ( 0.000000000000000000, 0.000000000000000000, -1.000000000000000000 ) ) ;
#594 = CARTESIAN_POINT ( 'NONE',  ( -30.80918829504999934, 27.97290950744599769, 64.35000000000000853 ) ) ;
#595 = CARTESIAN_POINT ( 'NONE',  ( 0.000000000000000000, 8.500000000000000000, 0.000000000000000000 ) ) ;
#596 = CARTESIAN_POINT ( 'NONE',  ( -25.67727386805000123, 10.97290950744599947, 61.65955166399999854 ) ) ;
#597 = APPLICATION_PROTOCOL_DEFINITION ( 'draft international standard', 'automotive_design', 1998, #9748 ) ;
#598 = CIRCLE ( 'NONE', #5937, 17.00000000000000355 ) ;
#599 = EDGE_CURVE ( 'NONE', #821, #11310, #9518, .T. ) ;
#600 = CYLINDRICAL_SURFACE ( 'NONE', #3494, 10.00000000000000178 ) ;
#601 = DIRECTION ( 'NONE',  ( 0.000000000000000000, 0.000000000000000000, 1.000000000000000000 ) ) ;
#602 = ORIENTED_EDGE ( 'NONE', *, *, #381, .T. ) ;
#603 = CARTESIAN_POINT ( 'NONE',  ( -1.059188295049996231, 27.97290950744599769, 58.85000000000000142 ) ) ;
#604 = DIRECTION ( 'NONE',  ( 0.000000000000000000, 0.000000000000000000, 1.000000000000000000 ) ) ;
#605 = CARTESIAN_POINT ( 'NONE',  ( -10.38347696868452097, 26.08535324214045303, 57.35000000000000142 ) ) ;
#606 = CARTESIAN_POINT ( 'NONE',  ( -18.05918829504999934, 10.97290950744599947, 118.8499999999999943 ) ) ;
#607 = DIRECTION ( 'NONE',  ( -1.000000000000000000, -1.239088197126292296E-16, -0.000000000000000000 ) ) ;
#608 = PLANE ( 'NONE',  #5540 ) ;
#609 = DIRECTION ( 'NONE',  ( 0.000000000000000000, 0.000000000000000000, -1.000000000000000000 ) ) ;
#610 = CARTESIAN_POINT ( 'NONE',  ( 50.63563590245420443, 94.90549801902425031, 22.75000000000000000 ) ) ;
#611 = CARTESIAN_POINT ( 'NONE',  ( -18.05918829504999934, 10.97290950744599947, 23.90000000000000213 ) ) ;
#612 = CARTESIAN_POINT ( 'NONE',  ( 140.6356359024541973, 108.9054980190242503, 20.00000000000000000 ) ) ;
#613 = AXIS2_PLACEMENT_3D ( 'NONE', #13711, #12870, #3257 ) ;
#614 = CIRCLE ( 'NONE', #1290, 1.999999999999998890 ) ;
#615 = EDGE_LOOP ( 'NONE', ( #433, #3515 ) ) ;
#616 = EDGE_CURVE ( 'NONE', #1958, #10012, #1673, .T. ) ;
#617 = DIRECTION ( 'NONE',  ( 1.000000000000000000, 0.000000000000000000, 0.000000000000000000 ) ) ;
#618 = EDGE_LOOP ( 'NONE', ( #4297, #9281, #12104, #1831, #7193, #7570, #5316, #11054, #1342, #8855, #9171, #9443, #11118, #5927, #3897, #4500 ) ) ;
#619 = ORIENTED_EDGE ( 'NONE', *, *, #11776, .F. ) ;
#620 = CARTESIAN_POINT ( 'NONE',  ( 134.7391892930474739, 104.0090514096174843, 23.00000000000000000 ) ) ;
#621 = DIRECTION ( 'NONE',  ( -0.000000000000000000, 1.000000000000000000, -0.000000000000000000 ) ) ;
#622 = FACE_OUTER_BOUND ( 'NONE', #303, .T. ) ;
#623 = VECTOR ( 'NONE', #10124, 1000.000000000000000 ) ;
#624 = DIRECTION ( 'NONE',  ( 0.000000000000000000, 0.000000000000000000, 1.000000000000000000 ) ) ;
#625 = AXIS2_PLACEMENT_3D ( 'NONE', #11625, #6317, #6376 ) ;
#626 = CARTESIAN_POINT ( 'NONE',  ( -34.49120980104999035, 2.756898754446010180, 63.36264408499989287 ) ) ;
#627 = DIRECTION ( 'NONE',  ( -0.000000000000000000, -0.000000000000000000, -1.000000000000000000 ) ) ;
#628 = CYLINDRICAL_SURFACE ( 'NONE', #4795, 6.449999999999997513 ) ;
#629 = ADVANCED_FACE ( 'NONE', ( #13264 ), #1537, .T. ) ;
#630 = AXIS2_PLACEMENT_3D ( 'NONE', #3794, #7899, #5933 ) ;
#631 = ORIENTED_EDGE ( 'NONE', *, *, #12993, .T. ) ;
#632 = ADVANCED_FACE ( 'NONE', ( #10206 ), #9225, .F. ) ;
#633 = CIRCLE ( 'NONE', #10686, 12.00000000000000355 ) ;
#634 = ORIENTED_EDGE ( 'NONE', *, *, #2585, .F. ) ;
#635 = CARTESIAN_POINT ( 'NONE',  ( -15.98447378135880292, 30.26743272304607402, 61.00728932202151356 ) ) ;
#636 = EDGE_CURVE ( 'NONE', #6971, #6593, #6837, .T. ) ;
#637 = ORIENTED_EDGE ( 'NONE', *, *, #12632, .F. ) ;
#638 = ORIENTED_EDGE ( 'NONE', *, *, #6718, .T. ) ;
#639 = CARTESIAN_POINT ( 'NONE',  ( -46.97970805730049904, -0.1071066662815775977, 64.85000000000000853 ) ) ;
#640 = CARTESIAN_POINT ( 'NONE',  ( -32.37473156004999453, 18.13068114044599710, 61.70038048200006386 ) ) ;
#641 = LINE ( 'NONE', #12326, #4442 ) ;
#642 = VERTEX_POINT ( 'NONE', #12160 ) ;
#643 = CARTESIAN_POINT ( 'NONE',  ( 0.09777679598749920709, -1.420146627243660031, 64.85000000000000853 ) ) ;
#644 = DIRECTION ( 'NONE',  ( 1.000000000000000000, 0.000000000000000000, 0.000000000000000000 ) ) ;
#645 = VECTOR ( 'NONE', #9718, 1000.000000000000000 ) ;
#646 = CIRCLE ( 'NONE', #2677, 0.5000000000000004441 ) ;
#647 = CARTESIAN_POINT ( 'NONE',  ( -16.74984313037099781, 27.92258346524268475, 58.10825715175638351 ) ) ;
#648 = CIRCLE ( 'NONE', #4894, 6.595833333000001630 ) ;
#649 = DIRECTION ( 'NONE',  ( 0.000000000000000000, 0.000000000000000000, -1.000000000000000000 ) ) ;
#650 = ADVANCED_FACE ( 'NONE', ( #11110 ), #5788, .F. ) ;
#651 = VERTEX_POINT ( 'NONE', #8027 ) ;
#652 = ORIENTED_EDGE ( 'NONE', *, *, #9198, .T. ) ;
#653 = CIRCLE ( 'NONE', #8245, 18.00000000000000000 ) ;
#654 = CARTESIAN_POINT ( 'NONE',  ( 4.500000000000002665, -0.5000000000000005551, 0.000000000000000000 ) ) ;
#655 = FACE_OUTER_BOUND ( 'NONE', #13439, .T. ) ;
#656 = LINE ( 'NONE', #12543, #7857 ) ;
#657 = LINE ( 'NONE', #12469, #5078 ) ;
#658 = DIRECTION ( 'NONE',  ( -1.000000000000000000, 0.000000000000000000, 0.000000000000000000 ) ) ;
#659 = DIRECTION ( 'NONE',  ( 0.000000000000000000, 0.000000000000000000, -1.000000000000000000 ) ) ;
#660 = DIRECTION ( 'NONE',  ( -1.000000000000000000, -6.780744947014009727E-15, 0.000000000000000000 ) ) ;
#661 = AXIS2_PLACEMENT_3D ( 'NONE', #13156, #2499, #314 ) ;
#662 = EDGE_CURVE ( 'NONE', #12520, #2653, #11388, .T. ) ;
#663 = ADVANCED_FACE ( 'NONE', ( #3779 ), #498, .F. ) ;
#664 = DIRECTION ( 'NONE',  ( -0.000000000000000000, -0.000000000000000000, -1.000000000000000000 ) ) ;
#665 = VERTEX_POINT ( 'NONE', #12304 ) ;
#666 = ORIENTED_EDGE ( 'NONE', *, *, #3497, .T. ) ;
#667 = CARTESIAN_POINT ( 'NONE',  ( 116.7775623211734342, 75.03908161011133870, 19.25000000000000000 ) ) ;
#668 = CARTESIAN_POINT ( 'NONE',  ( -32.35918829505000360, 27.97290950744599769, 58.85000000000000142 ) ) ;
#669 = EDGE_CURVE ( 'NONE', #8809, #5925, #7950, .T. ) ;
#670 = DIRECTION ( 'NONE',  ( 0.000000000000000000, 0.000000000000000000, -1.000000000000000000 ) ) ;
#671 = DIRECTION ( 'NONE',  ( -1.000000000000000000, 0.000000000000000000, 0.000000000000000000 ) ) ;
#672 = AXIS2_PLACEMENT_3D ( 'NONE', #7930, #1510, #1232 ) ;
#673 = AXIS2_PLACEMENT_3D ( 'NONE', #3504, #2473, #9929 ) ;
#674 = VECTOR ( 'NONE', #141, 1000.000000000000000 ) ;
#675 = CARTESIAN_POINT ( 'NONE',  ( 42.63563590245419732, 111.0390816101113387, 19.25000000000000000 ) ) ;
#676 = DIRECTION ( 'NONE',  ( 1.000000000000000000, 0.000000000000000000, 0.000000000000000000 ) ) ;
#677 = AXIS2_PLACEMENT_3D ( 'NONE', #13631, #848, #1908 ) ;
#678 = DIRECTION ( 'NONE',  ( 0.000000000000000000, 0.000000000000000000, 1.000000000000000000 ) ) ;
#679 = DIRECTION ( 'NONE',  ( 0.000000000000000000, -1.000000000000000000, 0.000000000000000000 ) ) ;
#680 = DIRECTION ( 'NONE',  ( 1.000000000000000000, 0.000000000000000000, 0.000000000000000000 ) ) ;
#681 = PRODUCT_DEFINITION_CONTEXT ( 'detailed design', #3608, 'design' ) ;
#682 = AXIS2_PLACEMENT_3D ( 'NONE', #4209, #2406, #6504 ) ;
#683 = VECTOR ( 'NONE', #6615, 1000.000000000000000 ) ;
#684 = VECTOR ( 'NONE', #328, 1000.000000000000000 ) ;
#685 = ORIENTED_EDGE ( 'NONE', *, *, #926, .F. ) ;
#686 = DIRECTION ( 'NONE',  ( 0.000000000000000000, 1.000000000000000000, 0.000000000000000000 ) ) ;
#687 = DIRECTION ( 'NONE',  ( 1.000000000000000000, 0.000000000000000000, 0.000000000000000000 ) ) ;
#688 = EDGE_CURVE ( 'NONE', #1735, #8958, #13408, .T. ) ;
#689 = FACE_BOUND ( 'NONE', #573, .T. ) ;
#690 = CYLINDRICAL_SURFACE ( 'NONE', #8513, 6.449999999999997513 ) ;
#691 = LINE ( 'NONE', #9361, #8209 ) ;
#692 = AXIS2_PLACEMENT_3D ( 'NONE', #1538, #7951, #7885 ) ;
#693 = AXIS2_PLACEMENT_3D ( 'NONE', #7006, #13442, #12398 ) ;
#694 = FACE_OUTER_BOUND ( 'NONE', #1462, .T. ) ;
#695 = AXIS2_PLACEMENT_3D ( 'NONE', #7919, #9259, #8346 ) ;
#696 = DIRECTION ( 'NONE',  ( 0.000000000000000000, 0.000000000000000000, 1.000000000000000000 ) ) ;
#697 = DIRECTION ( 'NONE',  ( 0.000000000000000000, 0.000000000000000000, 1.000000000000000000 ) ) ;
#698 = AXIS2_PLACEMENT_3D ( 'NONE', #6763, #12980, #13188 ) ;
#699 = ORIENTED_EDGE ( 'NONE', *, *, #2777, .F. ) ;
#700 = CARTESIAN_POINT ( 'NONE',  ( -15.26994104352865023, 30.19221003217483101, 60.32689770076000713 ) ) ;
#701 = ADVANCED_FACE ( 'NONE', ( #12089 ), #8706, .T. ) ;
#702 = ORIENTED_EDGE ( 'NONE', *, *, #5578, .T. ) ;
#703 = VERTEX_POINT ( 'NONE', #12706 ) ;
#704 = FACE_OUTER_BOUND ( 'NONE', #6355, .T. ) ;
#705 = LINE ( 'NONE', #2058, #9615 ) ;
#706 = ORIENTED_EDGE ( 'NONE', *, *, #11105, .T. ) ;
#707 = VERTEX_POINT ( 'NONE', #6065 ) ;
#708 = DIRECTION ( 'NONE',  ( 0.000000000000000000, 0.000000000000000000, 1.000000000000000000 ) ) ;
#709 = DIRECTION ( 'NONE',  ( 0.000000000000000000, 0.000000000000000000, -1.000000000000000000 ) ) ;
#710 = CYLINDRICAL_SURFACE ( 'NONE', #2943, 0.2500000000000002220 ) ;
#711 = DIRECTION ( 'NONE',  ( 0.000000000000000000, 0.000000000000000000, 1.000000000000000000 ) ) ;
#712 = EDGE_CURVE ( 'NONE', #11588, #3512, #7345, .T. ) ;
#713 = CARTESIAN_POINT ( 'NONE',  ( 44.63563590245420443, 103.9054980190242361, 20.00000000000000000 ) ) ;
#714 = EDGE_CURVE ( 'NONE', #95, #9971, #5288, .T. ) ;
#715 = DIRECTION ( 'NONE',  ( 0.7071067811865382469, -0.7071067811865567876, 0.000000000000000000 ) ) ;
#716 = AXIS2_PLACEMENT_3D ( 'NONE', #8147, #3761, #12356 ) ;
#717 = ORIENTED_EDGE ( 'NONE', *, *, #9515, .F. ) ;
#718 = EDGE_CURVE ( 'NONE', #999, #11456, #9839, .T. ) ;
#719 = VERTEX_POINT ( 'NONE', #10474 ) ;
#720 = ORIENTED_EDGE ( 'NONE', *, *, #2109, .T. ) ;
#721 = VERTEX_POINT ( 'NONE', #11382 ) ;
#722 = VERTEX_POINT ( 'NONE', #5224 ) ;
#723 = ORIENTED_EDGE ( 'NONE', *, *, #3044, .T. ) ;
#724 = EDGE_LOOP ( 'NONE', ( #8738, #2157, #10866, #9680 ) ) ;
#725 = CARTESIAN_POINT ( 'NONE',  ( -10.89348439749693931, -4.443078545630354981, 62.14999999999999858 ) ) ;
#726 = DIRECTION ( 'NONE',  ( 1.000000000000000000, 0.000000000000000000, 0.000000000000000000 ) ) ;
#727 = DIRECTION ( 'NONE',  ( 0.000000000000000000, 0.000000000000000000, -1.000000000000000000 ) ) ;
#728 = DIRECTION ( 'NONE',  ( 0.000000000000000000, 1.000000000000000000, 0.000000000000000000 ) ) ;
#729 = CARTESIAN_POINT ( 'NONE',  ( -18.05918829504999934, 10.97290950744599947, 11.50000000000000000 ) ) ;
#730 = EDGE_CURVE ( 'NONE', #12176, #10198, #9359, .T. ) ;
#731 = FACE_BOUND ( 'NONE', #2240, .T. ) ;
#732 = APPLICATION_PROTOCOL_DEFINITION ( 'draft international standard', 'automotive_design', 1998, #7861 ) ;
#733 = ORIENTED_EDGE ( 'NONE', *, *, #8919, .F. ) ;
#734 = EDGE_CURVE ( 'NONE', #8809, #7757, #3151, .T. ) ;
#735 = ORIENTED_EDGE ( 'NONE', *, *, #3847, .F. ) ;
#736 = EDGE_CURVE ( 'NONE', #4755, #1534, #2879, .T. ) ;
#737 = CIRCLE ( 'NONE', #12119, 2.700000000000000178 ) ;
#738 = PRODUCT_DEFINITION ( 'UNKNOWN', '', #8446, #5982 ) ;
#739 = EDGE_CURVE ( 'NONE', #9938, #3923, #2277, .T. ) ;
#740 = LINE ( 'NONE', #11291, #13292 ) ;
#741 = ORIENTED_EDGE ( 'NONE', *, *, #9101, .T. ) ;
#742 = CARTESIAN_POINT ( 'NONE',  ( -22.02876472382295248, 15.47207198241065029, 64.85000000000000853 ) ) ;
#743 = DIRECTION ( 'NONE',  ( 0.4528443260392608916, 0.8915896008669279560, 0.000000000000000000 ) ) ;
#744 = AXIS2_PLACEMENT_3D ( 'NONE', #7799, #6965, #281 ) ;
#745 = DIRECTION ( 'NONE',  ( -0.000000000000000000, -0.000000000000000000, -1.000000000000000000 ) ) ;
#746 = DIRECTION ( 'NONE',  ( 0.000000000000000000, -0.000000000000000000, 1.000000000000000000 ) ) ;
#747 = DIRECTION ( 'NONE',  ( -1.000000000000000000, 0.000000000000000000, 0.000000000000000000 ) ) ;
#748 = DIRECTION ( 'NONE',  ( -0.000000000000000000, -0.000000000000000000, -1.000000000000000000 ) ) ;
#749 = CYLINDRICAL_SURFACE ( 'NONE', #1816, 1.999999999999994893 ) ;
#750 = ADVANCED_FACE ( 'NONE', ( #8166 ), #4053, .F. ) ;
#751 = DIRECTION ( 'NONE',  ( 0.4528443260392610026, 0.8915896008669277339, 0.000000000000000000 ) ) ;
#752 = CARTESIAN_POINT ( 'NONE',  ( -25.33503448090910126, -7.245613863947209410, 68.85549045786049760 ) ) ;
#753 = EDGE_CURVE ( 'NONE', #8302, #651, #10078, .T. ) ;
#754 = EDGE_CURVE ( 'NONE', #707, #12928, #8309, .T. ) ;
#755 = VERTEX_POINT ( 'NONE', #6196 ) ;
#756 = ORIENTED_EDGE ( 'NONE', *, *, #234, .F. ) ;
#757 = CARTESIAN_POINT ( 'NONE',  ( 68.49370948373500312, 123.0390816101113245, 19.25000000000000000 ) ) ;
#758 = ORIENTED_EDGE ( 'NONE', *, *, #5194, .F. ) ;
#759 = VERTEX_POINT ( 'NONE', #5020 ) ;
#760 = ORIENTED_EDGE ( 'NONE', *, *, #5002, .F. ) ;
#761 = ORIENTED_EDGE ( 'NONE', *, *, #2809, .F. ) ;
#762 = CARTESIAN_POINT ( 'NONE',  ( -18.05918829504999934, 10.97290950744599947, 57.54999999999999716 ) ) ;
#763 = CARTESIAN_POINT ( 'NONE',  ( -18.05918829504999934, 10.97290950744599947, 64.85000000000000853 ) ) ;
#764 = ORIENTED_EDGE ( 'NONE', *, *, #8126, .F. ) ;
#765 = DIRECTION ( 'NONE',  ( 1.000000000000000000, 0.000000000000000000, 0.000000000000000000 ) ) ;
#766 = CARTESIAN_POINT ( 'NONE',  ( -28.87730642030694739, 29.81324547859995278, 17.25000000000000000 ) ) ;
#767 = EDGE_CURVE ( 'NONE', #7051, #13581, #9290, .T. ) ;
#768 = CARTESIAN_POINT ( 'NONE',  ( -10.47404583389237942, 25.90703532196704728, 61.85000000000000142 ) ) ;
#769 = FACE_OUTER_BOUND ( 'NONE', #2166, .T. ) ;
#770 = EDGE_CURVE ( 'NONE', #2779, #11622, #3159, .T. ) ;
#771 = ORIENTED_EDGE ( 'NONE', *, *, #9810, .F. ) ;
#772 = ORIENTED_EDGE ( 'NONE', *, *, #10939, .F. ) ;
#773 = CARTESIAN_POINT ( 'NONE',  ( -14.47298380915872329, 30.08178984978628279, 55.82826930748674243 ) ) ;
#774 = EDGE_LOOP ( 'NONE', ( #9428, #4976, #4421, #4256 ) ) ;
#775 = ORIENTED_EDGE ( 'NONE', *, *, #5852, .F. ) ;
#776 = LINE ( 'NONE', #13553, #11837 ) ;
#777 = CARTESIAN_POINT ( 'NONE',  ( -27.15409092487699994, 0.3335619008453594714, 62.14999999999999858 ) ) ;
#778 = ORIENTED_EDGE ( 'NONE', *, *, #4763, .F. ) ;
#779 = ORIENTED_EDGE ( 'NONE', *, *, #1207, .F. ) ;
#780 = DIRECTION ( 'NONE',  ( -0.000000000000000000, 1.000000000000000000, -0.000000000000000000 ) ) ;
#781 = DIRECTION ( 'NONE',  ( -0.3132098788326352912, -0.9496839325805432885, 0.000000000000000000 ) ) ;
#782 = DIRECTION ( 'NONE',  ( 1.000000000000000000, 0.000000000000000000, 0.000000000000000000 ) ) ;
#783 = DIRECTION ( 'NONE',  ( -1.000000000000000000, 0.000000000000000000, 0.000000000000000000 ) ) ;
#784 = DIRECTION ( 'NONE',  ( -1.000000000000000000, 0.000000000000000000, 0.000000000000000000 ) ) ;
#785 = DIRECTION ( 'NONE',  ( 0.000000000000000000, 0.000000000000000000, 1.000000000000000000 ) ) ;
#786 = VECTOR ( 'NONE', #7174, 1000.000000000000000 ) ;
#787 = EDGE_LOOP ( 'NONE', ( #3326, #3499 ) ) ;
#788 = ORIENTED_EDGE ( 'NONE', *, *, #13319, .F. ) ;
#789 = EDGE_CURVE ( 'NONE', #2553, #2266, #4127, .T. ) ;
#790 = ORIENTED_EDGE ( 'NONE', *, *, #753, .T. ) ;
#791 = DIRECTION ( 'NONE',  ( 0.000000000000000000, 0.000000000000000000, 1.000000000000000000 ) ) ;
#792 = AXIS2_PLACEMENT_3D ( 'NONE', #38, #8552, #2020 ) ;
#793 = CARTESIAN_POINT ( 'NONE',  ( -37.75918829505000218, -6.027090492554000534, 7.250000000000000000 ) ) ;
#794 = CARTESIAN_POINT ( 'NONE',  ( -18.05918829504999934, 10.97290950744599947, 61.86500000000000199 ) ) ;
#795 = CYLINDRICAL_SURFACE ( 'NONE', #10653, 4.250000000000000000 ) ;
#796 = FACE_OUTER_BOUND ( 'NONE', #2619, .T. ) ;
#797 = DIRECTION ( 'NONE',  ( 0.000000000000000000, 0.000000000000000000, 1.000000000000000000 ) ) ;
#798 = APPLICATION_PROTOCOL_DEFINITION ( 'draft international standard', 'automotive_design', 1998, #9304 ) ;
#799 = ORIENTED_EDGE ( 'NONE', *, *, #2109, .F. ) ;
#800 = AXIS2_PLACEMENT_3D ( 'NONE', #3403, #6591, #6800 ) ;
#801 = ADVANCED_FACE ( 'NONE', ( #1892 ), #7178, .F. ) ;
#802 = CARTESIAN_POINT ( 'NONE',  ( 112.1804561881462945, 85.03908161011133870, 20.00000000000000000 ) ) ;
#803 = VERTEX_POINT ( 'NONE', #7376 ) ;
#804 = EDGE_LOOP ( 'NONE', ( #9625, #4091 ) ) ;
#805 = LINE ( 'NONE', #3755, #462 ) ;
#806 = FACE_OUTER_BOUND ( 'NONE', #11782, .T. ) ;
#807 = DIRECTION ( 'NONE',  ( 0.000000000000000000, -1.000000000000000000, 0.000000000000000000 ) ) ;
#808 = DIRECTION ( 'NONE',  ( 0.000000000000000000, 0.000000000000000000, 1.000000000000000000 ) ) ;
#809 = DIRECTION ( 'NONE',  ( -0.000000000000000000, -1.000000000000000000, -0.000000000000000000 ) ) ;
#810 = DIRECTION ( 'NONE',  ( 0.000000000000000000, 0.000000000000000000, 1.000000000000000000 ) ) ;
#811 = FACE_OUTER_BOUND ( 'NONE', #12970, .T. ) ;
#812 = STYLED_ITEM ( 'NONE', ( #8523 ), #8946 ) ;
#813 = DIRECTION ( 'NONE',  ( 0.6615960714621564875, -0.7498604124941129490, 0.000000000000000000 ) ) ;
#814 = FILL_AREA_STYLE_COLOUR ( '', #12680 ) ;
#815 = ORIENTED_EDGE ( 'NONE', *, *, #331, .F. ) ;
#816 = EDGE_CURVE ( 'NONE', #1026, #1798, #3028, .T. ) ;
#817 = VECTOR ( 'NONE', #10677, 1000.000000000000000 ) ;
#818 = CARTESIAN_POINT ( 'NONE',  ( 50.38563590245420443, 104.1554980190242361, 23.00000000000000000 ) ) ;
#819 = ORIENTED_EDGE ( 'NONE', *, *, #1738, .F. ) ;
#820 = EDGE_CURVE ( 'NONE', #10863, #8191, #7815, .T. ) ;
#821 = VERTEX_POINT ( 'NONE', #7238 ) ;
#822 = ORIENTED_EDGE ( 'NONE', *, *, #13532, .F. ) ;
#823 = DIRECTION ( 'NONE',  ( 0.000000000000000000, 0.000000000000000000, 1.000000000000000000 ) ) ;
#824 = DIRECTION ( 'NONE',  ( 0.000000000000000000, 0.000000000000000000, -1.000000000000000000 ) ) ;
#825 = SURFACE_SIDE_STYLE ('',( #2881 ) ) ;
#826 = VERTEX_POINT ( 'NONE', #11517 ) ;
#827 = DIRECTION ( 'NONE',  ( 0.000000000000000000, 0.000000000000000000, 1.000000000000000000 ) ) ;
#828 = EDGE_CURVE ( 'NONE', #4114, #7318, #4718, .T. ) ;
#829 = CARTESIAN_POINT ( 'NONE',  ( 44.76431555889458025, 85.34974178189114014, 20.00000000000000000 ) ) ;
#830 = CARTESIAN_POINT ( 'NONE',  ( 105.4499059006094654, 83.97306027416853169, 20.00000000000000000 ) ) ;
#831 = AXIS2_PLACEMENT_3D ( 'NONE', #2439, #13238, #7776 ) ;
#832 = ORIENTED_EDGE ( 'NONE', *, *, #10912, .T. ) ;
#833 = ADVANCED_FACE ( 'NONE', ( #2460 ), #12829, .F. ) ;
#834 = CARTESIAN_POINT ( 'NONE',  ( -14.45668717981020457, 30.07924626547106683, 55.87780969119025087 ) ) ;
#835 = CIRCLE ( 'NONE', #2430, 8.250000000000001776 ) ;
#836 = ORIENTED_EDGE ( 'NONE', *, *, #6900, .F. ) ;
#837 = AXIS2_PLACEMENT_3D ( 'NONE', #9903, #13096, #3544 ) ;
#838 = ORIENTED_EDGE ( 'NONE', *, *, #4604, .F. ) ;
#839 = EDGE_LOOP ( 'NONE', ( #1003, #10345, #8315, #8505 ) ) ;
#840 = LINE ( 'NONE', #4002, #9289 ) ;
#841 = AXIS2_PLACEMENT_3D ( 'NONE', #2225, #1215, #100 ) ;
#842 = DIRECTION ( 'NONE',  ( -1.000000000000000000, 0.000000000000000000, 0.000000000000000000 ) ) ;
#843 = CARTESIAN_POINT ( 'NONE',  ( -18.05918829505001000, 2.755752219877027009, 63.35000000030875356 ) ) ;
#844 = ORIENTED_EDGE ( 'NONE', *, *, #10998, .T. ) ;
#845 = DIRECTION ( 'NONE',  ( -1.000000000000000000, 0.000000000000000000, 0.000000000000000000 ) ) ;
#846 = CARTESIAN_POINT ( 'NONE',  ( -35.05918829505000645, -6.027090492554000534, 17.25000000000000000 ) ) ;
#847 = EDGE_CURVE ( 'NONE', #13286, #11868, #12517, .T. ) ;
#848 = DIRECTION ( 'NONE',  ( 0.000000000000000000, 0.000000000000000000, -1.000000000000000000 ) ) ;
#849 = CARTESIAN_POINT ( 'NONE',  ( 2.262399129208274573, -0.4981161769137525952, 5.250000000000000000 ) ) ;
#850 = CARTESIAN_POINT ( 'NONE',  ( -6.600216501174579697, -2.179141222803619993, 62.14999999999999858 ) ) ;
#851 = LINE ( 'NONE', #7260, #13582 ) ;
#852 = AXIS2_PLACEMENT_3D ( 'NONE', #4821, #3857, #4429 ) ;
#853 = VECTOR ( 'NONE', #4362, 1000.000000000000000 ) ;
#854 = AXIS2_PLACEMENT_3D ( 'NONE', #5360, #1035, #3352 ) ;
#855 = VECTOR ( 'NONE', #2074, 999.9999999999998863 ) ;
#856 = ORIENTED_EDGE ( 'NONE', *, *, #4667, .F. ) ;
#857 = ORIENTED_EDGE ( 'NONE', *, *, #1780, .T. ) ;
#858 = ORIENTED_EDGE ( 'NONE', *, *, #13569, .T. ) ;
#859 = VERTEX_POINT ( 'NONE', #5564 ) ;
#860 = CIRCLE ( 'NONE', #13355, 1.725000000000000755 ) ;
#862 = ORIENTED_EDGE ( 'NONE', *, *, #3092, .T. ) ;
#861 = CIRCLE ( 'NONE', #5312, 13.50000000000000000 ) ;
#863 = DIRECTION ( 'NONE',  ( 0.000000000000000000, 0.000000000000000000, 1.000000000000000000 ) ) ;
#864 = AXIS2_PLACEMENT_3D ( 'NONE', #13755, #12657, #3296 ) ;
#865 = EDGE_CURVE ( 'NONE', #4986, #349, #9169, .T. ) ;
#866 = CARTESIAN_POINT ( 'NONE',  ( -19.16403910648224596, 30.33404188115190436, 61.52219105696395474 ) ) ;
#867 = FACE_OUTER_BOUND ( 'NONE', #7948, .T. ) ;
#868 = CARTESIAN_POINT ( 'NONE',  ( -13.40033457972183939, -4.525318844826149878, 62.14999999999999858 ) ) ;
#869 = CARTESIAN_POINT ( 'NONE',  ( 0.04028432657539351286, 4.500000000000000000, -20.54539866546728888 ) ) ;
#870 = CARTESIAN_POINT ( 'NONE',  ( 3.500000000000001776, 2.000000000000000000, -65.00000000000000000 ) ) ;
#871 =( BOUNDED_CURVE ( )  B_SPLINE_CURVE ( 3, ( #25, #9523, #5193, #3122 ),
 .UNSPECIFIED., .F., .F. ) 
 B_SPLINE_CURVE_WITH_KNOTS ( ( 4, 4 ),
 ( 1.570796326794896558, 3.141592653589793116 ),
 .UNSPECIFIED. ) 
 CURVE ( )  GEOMETRIC_REPRESENTATION_ITEM ( )  RATIONAL_B_SPLINE_CURVE ( ( 1.000000000000000000, 0.8047378541243649375, 0.8047378541243649375, 1.000000000000000000 ) ) 
 REPRESENTATION_ITEM ( '' )  );
#872 = CARTESIAN_POINT ( 'NONE',  ( 17.94081170494991184, 8.972909507445047339, 157.8500000000000512 ) ) ;
#873 = ORIENTED_EDGE ( 'NONE', *, *, #5532, .F. ) ;
#874 = EDGE_LOOP ( 'NONE', ( #7978, #8631 ) ) ;
#875 = AXIS2_PLACEMENT_3D ( 'NONE', #8204, #6101, #12403 ) ;
#876 = VECTOR ( 'NONE', #5241, 1000.000000000000000 ) ;
#877 = DIRECTION ( 'NONE',  ( 0.000000000000000000, 0.000000000000000000, -1.000000000000000000 ) ) ;
#878 = VERTEX_POINT ( 'NONE', #1235 ) ;
#879 = ORIENTED_EDGE ( 'NONE', *, *, #9126, .F. ) ;
#880 = DIRECTION ( 'NONE',  ( 0.000000000000000000, 0.000000000000000000, 1.000000000000000000 ) ) ;
#881 = LINE ( 'NONE', #10259, #7955 ) ;
#882 = PLANE ( 'NONE',  #7158 ) ;
#883 = CARTESIAN_POINT ( 'NONE',  ( 42.63563590245419732, 111.0390816101113103, 19.68933982822018081 ) ) ;
#884 = DIRECTION ( 'NONE',  ( 1.000000000000000000, 0.000000000000000000, 0.000000000000000000 ) ) ;
#885 = CARTESIAN_POINT ( 'NONE',  ( 103.4499059006094512, 83.97306027416853169, 10.00000000000000000 ) ) ;
#886 = FACE_OUTER_BOUND ( 'NONE', #3660, .T. ) ;
#887 = LINE ( 'NONE', #3967, #2339 ) ;
#888 = AXIS2_PLACEMENT_3D ( 'NONE', #11953, #2684, #6911 ) ;
#889 = CARTESIAN_POINT ( 'NONE',  ( 0.000000000000000000, 0.000000000000000000, 7.250000000000000000 ) ) ;
#890 = AXIS2_PLACEMENT_3D ( 'NONE', #8915, #4733, #3547 ) ;
#891 = ADVANCED_FACE ( 'NONE', ( #3224 ), #10819, .T. ) ;
#892 = EDGE_CURVE ( 'NONE', #1393, #10499, #12776, .T. ) ;
#893 = ORIENTED_EDGE ( 'NONE', *, *, #7390, .F. ) ;
#894 = ORIENTED_EDGE ( 'NONE', *, *, #7603, .F. ) ;
#895 = EDGE_LOOP ( 'NONE', ( #3869, #7424, #13659, #2544 ) ) ;
#896 = VECTOR ( 'NONE', #7716, 1000.000000000000000 ) ;
#897 = CARTESIAN_POINT ( 'NONE',  ( -40.33164489498319938, 10.97290950744599947, 17.25000000000000000 ) ) ;
#898 = VERTEX_POINT ( 'NONE', #7433 ) ;
#899 = ORIENTED_EDGE ( 'NONE', *, *, #1394, .F. ) ;
#900 = DIRECTION ( 'NONE',  ( -1.000000000000000000, 0.000000000000000000, 0.000000000000000000 ) ) ;
#901 = DIRECTION ( 'NONE',  ( 0.000000000000000000, 0.000000000000000000, 1.000000000000000000 ) ) ;
#902 = CARTESIAN_POINT ( 'NONE',  ( -41.50918829505000218, -6.027090492554000534, 5.250000000000000000 ) ) ;
#903 = CARTESIAN_POINT ( 'NONE',  ( -18.05918829504999934, 10.97290950744599947, 63.02000000000000313 ) ) ;
#904 = EDGE_CURVE ( 'NONE', #3647, #3770, #5487, .T. ) ;
#905 = AXIS2_PLACEMENT_3D ( 'NONE', #10351, #13424, #6008 ) ;
#906 = CIRCLE ( 'NONE', #8713, 3.000000000000002665 ) ;
#907 = CIRCLE ( 'NONE', #2271, 6.849999999999999645 ) ;
#908 = AXIS2_PLACEMENT_3D ( 'NONE', #3569, #4603, #5491 ) ;
#909 = ORIENTED_EDGE ( 'NONE', *, *, #1487, .F. ) ;
#910 = CARTESIAN_POINT ( 'NONE',  ( -14.60499646201505186, 30.10205818033629299, 59.22435544807014907 ) ) ;
#911 = ORIENTED_EDGE ( 'NONE', *, *, #332, .F. ) ;
#912 = VERTEX_POINT ( 'NONE', #6408 ) ;
#913 = DIRECTION ( 'NONE',  ( 0.000000000000000000, 0.000000000000000000, 1.000000000000000000 ) ) ;
#914 = CIRCLE ( 'NONE', #8279, 16.00000000000000000 ) ;
#915 = CARTESIAN_POINT ( 'NONE',  ( -11.71335496205000126, 10.97290950744599947, 60.40999999999999659 ) ) ;
#916 = VECTOR ( 'NONE', #2209, 1000.000000000000000 ) ;
#917 = PLANE ( 'NONE',  #4481 ) ;
#918 = VERTEX_POINT ( 'NONE', #6688 ) ;
#919 = ORIENTED_EDGE ( 'NONE', *, *, #9714, .F. ) ;
#920 = DIRECTION ( 'NONE',  ( 0.000000000000000000, 0.000000000000000000, 1.000000000000000000 ) ) ;
#921 = FACE_OUTER_BOUND ( 'NONE', #12157, .T. ) ;
#922 = ORIENTED_EDGE ( 'NONE', *, *, #6084, .T. ) ;
#923 = LINE ( 'NONE', #12005, #1345 ) ;
#924 = DIRECTION ( 'NONE',  ( 0.000000000000000000, 0.000000000000000000, -1.000000000000000000 ) ) ;
#925 = DIRECTION ( 'NONE',  ( 1.000000000000000000, 0.000000000000000000, 0.000000000000000000 ) ) ;
#926 = EDGE_CURVE ( 'NONE', #10303, #13667, #5427, .T. ) ;
#927 = DIRECTION ( 'NONE',  ( 1.000000000000000000, -1.792228749776983267E-15, 0.000000000000000000 ) ) ;
#928 = EDGE_CURVE ( 'NONE', #1230, #2349, #8492, .T. ) ;
#929 = AXIS2_PLACEMENT_3D ( 'NONE', #13132, #12161, #1467 ) ;
#930 = AXIS2_PLACEMENT_3D ( 'NONE', #2140, #27, #6855 ) ;
#931 = AXIS2_PLACEMENT_3D ( 'NONE', #5128, #13652, #4994 ) ;
#932 = ORIENTED_EDGE ( 'NONE', *, *, #13740, .F. ) ;
#933 = ORIENTED_EDGE ( 'NONE', *, *, #4165, .F. ) ;
#934 = ADVANCED_FACE ( 'NONE', ( #275 ), #5359, .T. ) ;
#935 = ORIENTED_EDGE ( 'NONE', *, *, #9064, .F. ) ;
#936 = VERTEX_POINT ( 'NONE', #9767 ) ;
#937 = EDGE_LOOP ( 'NONE', ( #8404, #3809, #12332, #11896 ) ) ;
#938 = ORIENTED_EDGE ( 'NONE', *, *, #296, .F. ) ;
#939 = VERTEX_POINT ( 'NONE', #8720 ) ;
#940 = DIRECTION ( 'NONE',  ( 0.000000000000000000, 0.000000000000000000, 1.000000000000000000 ) ) ;
#941 = PLANE ( 'NONE',  #5749 ) ;
#942 = CARTESIAN_POINT ( 'NONE',  ( -20.31624426159365626, 30.25036691372644881, 60.86381688408464896 ) ) ;
#943 = CIRCLE ( 'NONE', #11875, 2.700000000000000178 ) ;
#944 = DIRECTION ( 'NONE',  ( -0.000000000000000000, -0.000000000000000000, 1.000000000000000000 ) ) ;
#945 = FACE_OUTER_BOUND ( 'NONE', #6346, .T. ) ;
#946 = FACE_OUTER_BOUND ( 'NONE', #13280, .T. ) ;
#947 = ADVANCED_FACE ( 'NONE', ( #11786 ), #472, .F. ) ;
#948 = CARTESIAN_POINT ( 'NONE',  ( 68.49370948373500312, 113.0390816101113387, 19.25000000000000000 ) ) ;
#949 = CONTEXT_DEPENDENT_SHAPE_REPRESENTATION ( #2176, #2488 ) ;
#950 = ADVANCED_FACE ( 'NONE', ( #5636 ), #10890, .F. ) ;
#951 = AXIS2_PLACEMENT_3D ( 'NONE', #11850, #9687, #9544 ) ;
#952 = VERTEX_POINT ( 'NONE', #9701 ) ;
#953 = ORIENTED_EDGE ( 'NONE', *, *, #5603, .T. ) ;
#954 = DIRECTION ( 'NONE',  ( 0.000000000000000000, 0.000000000000000000, -1.000000000000000000 ) ) ;
#955 = DIRECTION ( 'NONE',  ( 0.000000000000000000, 0.000000000000000000, -1.000000000000000000 ) ) ;
#956 = VERTEX_POINT ( 'NONE', #4333 ) ;
#957 = LINE ( 'NONE', #5336, #4928 ) ;
#958 = CARTESIAN_POINT ( 'NONE',  ( 44.94629607423404849, 85.78908161011133870, 20.00000000000000000 ) ) ;
#959 = DIRECTION ( 'NONE',  ( -0.000000000000000000, -0.000000000000000000, 1.000000000000000000 ) ) ;
#960 =( BOUNDED_CURVE ( )  B_SPLINE_CURVE ( 3, ( #7023, #6960, #883, #675 ),
 .UNSPECIFIED., .F., .F. ) 
 B_SPLINE_CURVE_WITH_KNOTS ( ( 4, 4 ),
 ( 4.712388980384689674, 6.283185307179586232 ),
 .UNSPECIFIED. ) 
 CURVE ( )  GEOMETRIC_REPRESENTATION_ITEM ( )  RATIONAL_B_SPLINE_CURVE ( ( 1.000000000000000000, 0.8047378541243649375, 0.8047378541243649375, 1.000000000000000000 ) ) 
 REPRESENTATION_ITEM ( '' )  );
#961 = LINE ( 'NONE', #5143, #2985 ) ;
#962 = LINE ( 'NONE', #4945, #9540 ) ;
#963 = CARTESIAN_POINT ( 'NONE',  ( -18.05918829504999934, 10.97290950744599947, 17.25000000000000000 ) ) ;
#964 = DIRECTION ( 'NONE',  ( -1.000000000000000000, 0.000000000000000000, 0.000000000000000000 ) ) ;
#965 = AXIS2_PLACEMENT_3D ( 'NONE', #794, #4025, #1642 ) ;
#966 = LINE ( 'NONE', #11855, #9582 ) ;
#967 = FACE_BOUND ( 'NONE', #1057, .T. ) ;
#968 = ORIENTED_EDGE ( 'NONE', *, *, #7622, .F. ) ;
#969 = CIRCLE ( 'NONE', #4104, 5.000000000000000888 ) ;
#970 = ORIENTED_EDGE ( 'NONE', *, *, #2125, .T. ) ;
#971 = DIRECTION ( 'NONE',  ( -0.000000000000000000, -1.000000000000000000, -0.000000000000000000 ) ) ;
#972 = EDGE_CURVE ( 'NONE', #1552, #4825, #7152, .T. ) ;
#973 = VERTEX_POINT ( 'NONE', #11936 ) ;
#974 = ORIENTED_EDGE ( 'NONE', *, *, #3018, .T. ) ;
#975 = CARTESIAN_POINT ( 'NONE',  ( -20.72384131171161670, 15.28981433190530481, 68.77695026631712949 ) ) ;
#976 = ORIENTED_EDGE ( 'NONE', *, *, #1683, .F. ) ;
#977 = DIRECTION ( 'NONE',  ( -1.000000000000000000, 0.000000000000000000, 0.000000000000000000 ) ) ;
#978 = DIRECTION ( 'NONE',  ( 0.000000000000000000, 0.000000000000000000, 1.000000000000000000 ) ) ;
#979 = DIRECTION ( 'NONE',  ( 1.000000000000000000, 0.000000000000000000, 0.000000000000000000 ) ) ;
#980 = CARTESIAN_POINT ( 'NONE',  ( 134.7391892930474739, 94.80194462843097369, 23.00000000000000000 ) ) ;
#981 = AXIS2_PLACEMENT_3D ( 'NONE', #1980, #1903, #12787 ) ;
#982 = EDGE_CURVE ( 'NONE', #12299, #13004, #1126, .T. ) ;
#983 = EDGE_LOOP ( 'NONE', ( #822, #4361, #9939, #6406 ) ) ;
#984 = CARTESIAN_POINT ( 'NONE',  ( -14.25042417982650278, 30.04605120274296581, 56.81979108752121732 ) ) ;
#985 = EDGE_LOOP ( 'NONE', ( #2986, #6545, #13641, #7697 ) ) ;
#986 = EDGE_CURVE ( 'NONE', #8958, #194, #11849, .T. ) ;
#987 = ORIENTED_EDGE ( 'NONE', *, *, #12687, .F. ) ;
#988 = EDGE_LOOP ( 'NONE', ( #8522, #8841 ) ) ;
#989 = CARTESIAN_POINT ( 'NONE',  ( 43.38563590245419732, 87.34974178189119698, 0.000000000000000000 ) ) ;
#990 = PRESENTATION_STYLE_ASSIGNMENT (( #6217 ) ) ;
#991 = CARTESIAN_POINT ( 'NONE',  ( -10.81426999815532852, 15.06602133594271820, 0.000000000000000000 ) ) ;
#992 = CARTESIAN_POINT ( 'NONE',  ( -7.499999999999996447, -1.762812401309176307E-15, -65.00000000000000000 ) ) ;
#993 = CARTESIAN_POINT ( 'NONE',  ( -25.86749127492454647, -8.860076549334129581, 5.250000000000000000 ) ) ;
#994 = DIRECTION ( 'NONE',  ( 1.000000000000000000, 0.000000000000000000, 0.000000000000000000 ) ) ;
#995 = DIRECTION ( 'NONE',  ( -0.6615960714621568206, 0.7498604124941127269, 0.000000000000000000 ) ) ;
#996 = EDGE_LOOP ( 'NONE', ( #10152, #2242, #2087, #5658 ) ) ;
#997 = VERTEX_POINT ( 'NONE', #7721 ) ;
#998 = EDGE_CURVE ( 'NONE', #1834, #3793, #2322, .T. ) ;
#999 = VERTEX_POINT ( 'NONE', #9979 ) ;
#1000 = VERTEX_POINT ( 'NONE', #12281 ) ;
#1001 = CARTESIAN_POINT ( 'NONE',  ( -1.059188295049996231, 10.97290950744599947, 64.35000000000000853 ) ) ;
#1002 = DIRECTION ( 'NONE',  ( 1.224646799147353207E-16, 1.000000000000000000, -0.000000000000000000 ) ) ;
#1003 = ORIENTED_EDGE ( 'NONE', *, *, #3652, .F. ) ;
#1004 = DIRECTION ( 'NONE',  ( 0.000000000000000000, 0.000000000000000000, -1.000000000000000000 ) ) ;
#1005 = CARTESIAN_POINT ( 'NONE',  ( -17.78571402079797892, 26.97096642121225685, 55.86712588480680353 ) ) ;
#1006 = DIRECTION ( 'NONE',  ( 0.000000000000000000, 1.000000000000000000, 0.000000000000000000 ) ) ;
#1007 = DIRECTION ( 'NONE',  ( -1.000000000000000000, 0.000000000000000000, 0.000000000000000000 ) ) ;
#1008 = EDGE_CURVE ( 'NONE', #10778, #2084, #2802, .T. ) ;
#1009 = AXIS2_PLACEMENT_3D ( 'NONE', #10779, #9586, #6641 ) ;
#1010 = DIRECTION ( 'NONE',  ( 0.7071067811865500152, 0.000000000000000000, 0.7071067811865450192 ) ) ;
#1011 = ORIENTED_EDGE ( 'NONE', *, *, #12563, .F. ) ;
#1012 = ORIENTED_EDGE ( 'NONE', *, *, #11390, .T. ) ;
#1013 = ADVANCED_FACE ( 'NONE', ( #7022 ), #3760, .F. ) ;
#1014 = VECTOR ( 'NONE', #9490, 1000.000000000000000 ) ;
#1015 = DIRECTION ( 'NONE',  ( 1.000000000000000000, 0.000000000000000000, 0.000000000000000000 ) ) ;
#1016 = DIRECTION ( 'NONE',  ( 1.000000000000000000, 0.000000000000000000, 0.000000000000000000 ) ) ;
#1017 = DIRECTION ( 'NONE',  ( -0.000000000000000000, -0.000000000000000000, 1.000000000000000000 ) ) ;
#1018 = DIRECTION ( 'NONE',  ( 0.000000000000000000, 0.000000000000000000, -1.000000000000000000 ) ) ;
#1019 = FACE_OUTER_BOUND ( 'NONE', #11910, .T. ) ;
#1020 = DIRECTION ( 'NONE',  ( 0.000000000000000000, 1.000000000000000000, 0.000000000000000000 ) ) ;
#1021 = DIRECTION ( 'NONE',  ( 0.000000000000000000, 0.000000000000000000, -1.000000000000000000 ) ) ;
#1022 = CARTESIAN_POINT ( 'NONE',  ( -23.85417428574490373, 12.52794563810342154, 64.85000000000000853 ) ) ;
#1023 = ADVANCED_FACE ( 'NONE', ( #5698 ), #6891, .T. ) ;
#1024 = CARTESIAN_POINT ( 'NONE',  ( 68.49370948373500312, 75.03908161011133870, 20.00000000000000000 ) ) ;
#1025 = ORIENTED_EDGE ( 'NONE', *, *, #5478, .T. ) ;
#1026 = VERTEX_POINT ( 'NONE', #1656 ) ;
#1027 =( BOUNDED_SURFACE ( )  B_SPLINE_SURFACE ( 3, 3, ( 
 ( #12793, #11740, #6432, #2340 ),
 ( #9511, #10771, #1190, #8741 ),
 ( #3106, #13757, #7328, #8457 ),
 ( #2550, #11050, #12094, #7668 ) ),
 .UNSPECIFIED., .F., .F., .F. ) 
 B_SPLINE_SURFACE_WITH_KNOTS ( ( 4, 4 ),
 ( 4, 4 ),
 ( 0.000000000000000000, 1.000000000000000000 ),
 ( 0.000000000000000000, 1.000000000000000000 ),
 .UNSPECIFIED. ) 
 GEOMETRIC_REPRESENTATION_ITEM ( )  RATIONAL_B_SPLINE_SURFACE ( (
 ( 1.000000000000000000, 0.3333333333333329818, 0.3333333333333329818, 1.000000000000000000),
 ( 0.7553208711179729695, 0.2517736237059909898, 0.2517736237059909898, 0.7553208711179729695),
 ( 0.7553208711179729695, 0.2517736237059909898, 0.2517736237059909898, 0.7553208711179729695),
 ( 1.000000000000000000, 0.3333333333333329818, 0.3333333333333329818, 1.000000000000000000) ) ) 
 REPRESENTATION_ITEM ( '' )  SURFACE ( )  );
#1028 = CARTESIAN_POINT ( 'NONE',  ( 5.999999999999999112, 11.99999999999999822, 0.000000000000000000 ) ) ;
#1029 = ORIENTED_EDGE ( 'NONE', *, *, #10898, .T. ) ;
#1030 = ORIENTED_EDGE ( 'NONE', *, *, #428, .F. ) ;
#1031 = DIRECTION ( 'NONE',  ( 1.000000000000000000, 0.000000000000000000, 0.000000000000000000 ) ) ;
#1032 = AXIS2_PLACEMENT_3D ( 'NONE', #7320, #3174, #6360 ) ;
#1033 = DIRECTION ( 'NONE',  ( 0.7071067811865525687, 0.7071067811865425767, -0.000000000000000000 ) ) ;
#1034 = EDGE_LOOP ( 'NONE', ( #12440, #4018 ) ) ;
#1035 = DIRECTION ( 'NONE',  ( -0.000000000000000000, -0.000000000000000000, -1.000000000000000000 ) ) ;
#1036 = ADVANCED_FACE ( 'NONE', ( #10126 ), #4674, .F. ) ;
#1037 = CARTESIAN_POINT ( 'NONE',  ( -18.05918829504999934, 10.97290950744599947, 60.85000000000000142 ) ) ;
#1038 = EDGE_CURVE ( 'NONE', #10499, #510, #906, .T. ) ;
#1039 = CIRCLE ( 'NONE', #1255, 0.7500000000000000000 ) ;
#1040 = EDGE_LOOP ( 'NONE', ( #4955, #12743 ) ) ;
#1041 = DIRECTION ( 'NONE',  ( 1.000000000000000000, 0.000000000000000000, 0.000000000000000000 ) ) ;
#1042 = VERTEX_POINT ( 'NONE', #1724 ) ;
#1043 = ORIENTED_EDGE ( 'NONE', *, *, #8109, .F. ) ;
#1044 = CARTESIAN_POINT ( 'NONE',  ( 44.63563590245420443, 94.90549801902425031, 23.00000000000000000 ) ) ;
#1045 = CARTESIAN_POINT ( 'NONE',  ( 16.04064420431708982, 0.000000000000000000, 7.307586582922145801 ) ) ;
#1046 = DIRECTION ( 'NONE',  ( 1.000000000000000000, 0.000000000000000000, 0.000000000000000000 ) ) ;
#1047 = CYLINDRICAL_SURFACE ( 'NONE', #5313, 18.00000000000000000 ) ;
#1048 = AXIS2_PLACEMENT_3D ( 'NONE', #5562, #7652, #4535 ) ;
#1049 = DIRECTION ( 'NONE',  ( 0.000000000000000000, 0.000000000000000000, 1.000000000000000000 ) ) ;
#1050 = DIRECTION ( 'NONE',  ( 1.000000000000000000, 0.000000000000000000, 0.000000000000000000 ) ) ;
#1051 = EDGE_CURVE ( 'NONE', #13262, #13219, #7867, .T. ) ;
#1052 = EDGE_CURVE ( 'NONE', #3941, #217, #10504, .T. ) ;
#1053 = CIRCLE ( 'NONE', #4855, 2.000000000000001776 ) ;
#1054 = ORIENTED_EDGE ( 'NONE', *, *, #13308, .T. ) ;
#1055 = EDGE_LOOP ( 'NONE', ( #11743, #1398, #10361, #10586 ) ) ;
#1056 = DIRECTION ( 'NONE',  ( 1.000000000000000000, 0.000000000000000000, 0.000000000000000000 ) ) ;
#1057 = EDGE_LOOP ( 'NONE', ( #4199, #7252 ) ) ;
#1058 = ORIENTED_EDGE ( 'NONE', *, *, #8481, .T. ) ;
#1059 = ORIENTED_EDGE ( 'NONE', *, *, #7926, .T. ) ;
#1060 = EDGE_CURVE ( 'NONE', #5576, #1179, #12296, .T. ) ;
#1061 = DIRECTION ( 'NONE',  ( 0.000000000000000000, 0.000000000000000000, -1.000000000000000000 ) ) ;
#1062 = CARTESIAN_POINT ( 'NONE',  ( 140.6356359024541973, 103.9054980190242361, 22.75000000000000000 ) ) ;
#1063 = ORIENTED_EDGE ( 'NONE', *, *, #4240, .F. ) ;
#1064 = DIRECTION ( 'NONE',  ( 0.000000000000000000, 2.732534507816520408E-15, 1.000000000000000000 ) ) ;
#1065 = CIRCLE ( 'NONE', #852, 3.000000000000001332 ) ;
#1066 = DIRECTION ( 'NONE',  ( -2.267612386897784912E-16, 1.000000000000000000, 0.000000000000000000 ) ) ;
#1067 = AXIS2_PLACEMENT_3D ( 'NONE', #6316, #6958, #11232 ) ;
#1068 = FACE_OUTER_BOUND ( 'NONE', #8752, .T. ) ;
#1069 = VECTOR ( 'NONE', #11237, 1000.000000000000000 ) ;
#1070 = CYLINDRICAL_SURFACE ( 'NONE', #3179, 4.750000000000000888 ) ;
#1071 = CIRCLE ( 'NONE', #6425, 16.75000000000000355 ) ;
#1072 = DIRECTION ( 'NONE',  ( -1.000000000000000000, 0.000000000000000000, 0.000000000000000000 ) ) ;
#1073 = ORIENTED_EDGE ( 'NONE', *, *, #10346, .F. ) ;
#1074 = EDGE_CURVE ( 'NONE', #2266, #4291, #7792, .T. ) ;
#1075 =( GEOMETRIC_REPRESENTATION_CONTEXT ( 3 ) GLOBAL_UNCERTAINTY_ASSIGNED_CONTEXT ( ( #1813 ) ) GLOBAL_UNIT_ASSIGNED_CONTEXT ( ( #10879, #7487, #2162 ) ) REPRESENTATION_CONTEXT ( 'NONE', 'WORKASPACE' ) );
#1076 = VECTOR ( 'NONE', #13792, 1000.000000000000000 ) ;
#1077 = ORIENTED_EDGE ( 'NONE', *, *, #9933, .F. ) ;
#1078 = EDGE_LOOP ( 'NONE', ( #8229, #12932, #2407, #9421, #12105, #10029, #4887, #9297 ) ) ;
#1079 = ORIENTED_EDGE ( 'NONE', *, *, #4393, .F. ) ;
#1080 = VECTOR ( 'NONE', #13189, 1000.000000000000000 ) ;
#1081 = CARTESIAN_POINT ( 'NONE',  ( -18.05918829504999934, 10.97290950744599947, 64.85000000000000853 ) ) ;
#1082 = ORIENTED_EDGE ( 'NONE', *, *, #3973, .T. ) ;
#1083 = LINE ( 'NONE', #2086, #7729 ) ;
#1084 = CARTESIAN_POINT ( 'NONE',  ( 113.0903281124166710, 100.8715034839261762, 20.00000000000000000 ) ) ;
#1085 = DIRECTION ( 'NONE',  ( 0.000000000000000000, 0.000000000000000000, 1.000000000000000000 ) ) ;
#1086 = FACE_OUTER_BOUND ( 'NONE', #3397, .T. ) ;
#1087 = DIRECTION ( 'NONE',  ( 0.000000000000000000, 0.000000000000000000, 1.000000000000000000 ) ) ;
#1088 = CARTESIAN_POINT ( 'NONE',  ( -18.05918829505001355, 3.364325185446006117, 61.98378871700002435 ) ) ;
#1089 = CARTESIAN_POINT ( 'NONE',  ( -10.81426999815532852, 15.06602133594271820, 0.000000000000000000 ) ) ;
#1090 = LINE ( 'NONE', #7486, #2247 ) ;
#1091 = EDGE_CURVE ( 'NONE', #8284, #12316, #5585, .T. ) ;
#1092 = AXIS2_PLACEMENT_3D ( 'NONE', #8296, #4044, #1942 ) ;
#1093 = ADVANCED_FACE ( 'NONE', ( #8928 ), #13314, .T. ) ;
#1094 = ORIENTED_EDGE ( 'NONE', *, *, #12335, .T. ) ;
#1095 = CARTESIAN_POINT ( 'NONE',  ( -25.33503448090910126, 29.19143287883919768, 64.85000000000000853 ) ) ;
#1096 = ORIENTED_EDGE ( 'NONE', *, *, #5921, .F. ) ;
#1097 = CARTESIAN_POINT ( 'NONE',  ( 116.7775623211734342, 123.0390816101113245, 0.000000000000000000 ) ) ;
#1098 = DIRECTION ( 'NONE',  ( -1.000000000000000000, 5.059610138265691632E-16, 0.000000000000000000 ) ) ;
#1099 = CIRCLE ( 'NONE', #2017, 6.449999999999997513 ) ;
#1100 = CARTESIAN_POINT ( 'NONE',  ( 134.6356359024541973, 94.90549801902425031, 20.00000000000000000 ) ) ;
#1101 = CARTESIAN_POINT ( 'NONE',  ( -15.65757483969475139, 6.423926902242667047, 68.70888082541688391 ) ) ;
#1102 = DIRECTION ( 'NONE',  ( 0.000000000000000000, 0.000000000000000000, -1.000000000000000000 ) ) ;
#1103 = TOROIDAL_SURFACE ( 'NONE', #5141, 23.29163056034262169, 0.7500000000000000000 ) ;
#1104 = VECTOR ( 'NONE', #12608, 1000.000000000000000 ) ;
#1105 = ORIENTED_EDGE ( 'NONE', *, *, #143, .F. ) ;
#1106 = ADVANCED_FACE ( 'NONE', ( #9134 ), #6762, .F. ) ;
#1107 = CARTESIAN_POINT ( 'NONE',  ( -16.30182512297070829, 30.29372715573303054, 53.48163241110348309 ) ) ;
#1108 = VERTEX_POINT ( 'NONE', #3836 ) ;
#1109 = VERTEX_POINT ( 'NONE', #1449 ) ;
#1110 = FACE_OUTER_BOUND ( 'NONE', #6091, .T. ) ;
#1111 = DIRECTION ( 'NONE',  ( -1.000000000000000000, 0.000000000000000000, -0.000000000000000000 ) ) ;
#1112 = DIRECTION ( 'NONE',  ( 0.000000000000000000, 0.000000000000000000, -1.000000000000000000 ) ) ;
#1113 = DIRECTION ( 'NONE',  ( 1.000000000000000000, 0.000000000000000000, 0.000000000000000000 ) ) ;
#1114 = CARTESIAN_POINT ( 'NONE',  ( -43.05918829505001355, -11.02709049255400053, 0.000000000000000000 ) ) ;
#1115 = CIRCLE ( 'NONE', #672, 2.000000000000000000 ) ;
#1116 = AXIS2_PLACEMENT_3D ( 'NONE', #7517, #1325, #3440 ) ;
#1117 = AXIS2_PLACEMENT_3D ( 'NONE', #12921, #6570, #10841 ) ;
#1118 = CYLINDRICAL_SURFACE ( 'NONE', #3129, 16.72262947720610171 ) ;
#1119 = CARTESIAN_POINT ( 'NONE',  ( -37.05918829505000645, 29.97290950744599769, 64.85000000000000853 ) ) ;
#1120 = EDGE_CURVE ( 'NONE', #8521, #2257, #4929, .T. ) ;
#1121 = ORIENTED_EDGE ( 'NONE', *, *, #8680, .T. ) ;
#1122 = ORIENTED_EDGE ( 'NONE', *, *, #12876, .F. ) ;
#1123 = ORIENTED_EDGE ( 'NONE', *, *, #7029, .T. ) ;
#1124 = VECTOR ( 'NONE', #7353, 999.9999999999998863 ) ;
#1125 = DIRECTION ( 'NONE',  ( -1.000000000000000000, 0.000000000000000000, 0.000000000000000000 ) ) ;
#1126 = CIRCLE ( 'NONE', #10732, 24.03999999999999915 ) ;
#1127 = VECTOR ( 'NONE', #13305, 1000.000000000000000 ) ;
#1128 = VERTEX_POINT ( 'NONE', #8999 ) ;
#1129 = ORIENTED_EDGE ( 'NONE', *, *, #9612, .T. ) ;
#1130 = VERTEX_POINT ( 'NONE', #1513 ) ;
#1131 = ADVANCED_FACE ( 'NONE', ( #5769 ), #10054, .T. ) ;
#1132 = DIRECTION ( 'NONE',  ( 0.000000000000000000, 0.000000000000000000, -1.000000000000000000 ) ) ;
#1133 = EDGE_CURVE ( 'NONE', #7637, #11014, #11860, .T. ) ;
#1134 = CARTESIAN_POINT ( 'NONE',  ( -18.05918829504999934, 7.130333642789880244, 5.250000000000000000 ) ) ;
#1135 = EDGE_LOOP ( 'NONE', ( #7058, #3626, #8748, #2169 ) ) ;
#1136 = LINE ( 'NONE', #10578, #6722 ) ;
#1137 = CYLINDRICAL_SURFACE ( 'NONE', #11440, 4.749999999999997335 ) ;
#1138 = CARTESIAN_POINT ( 'NONE',  ( 44.63563590245422574, 112.2890816101113387, 20.00000000000000000 ) ) ;
#1139 = DIRECTION ( 'NONE',  ( -1.000000000000000000, 0.000000000000000000, 0.000000000000000000 ) ) ;
#1140 = CARTESIAN_POINT ( 'NONE',  ( -13.05918829504999756, 10.97290950744599947, 116.8499999999999943 ) ) ;
#1141 = AXIS2_PLACEMENT_3D ( 'NONE', #9226, #4896, #12642 ) ;
#1142 = AXIS2_PLACEMENT_3D ( 'NONE', #2025, #13458, #8422 ) ;
#1143 = PRODUCT_CONTEXT ( 'NONE', #8055, 'mechanical' ) ;
#1144 = ORIENTED_EDGE ( 'NONE', *, *, #5002, .T. ) ;
#1145 = VECTOR ( 'NONE', #13775, 1000.000000000000000 ) ;
#1146 = VERTEX_POINT ( 'NONE', #2090 ) ;
#1147 = PRESENTATION_LAYER_ASSIGNMENT (  '', '', ( #5381 ) ) ;
#1148 = CARTESIAN_POINT ( 'NONE',  ( -1.059188295049996231, -6.027090492554000534, 0.000000000000000000 ) ) ;
#1149 = FACE_OUTER_BOUND ( 'NONE', #5234, .T. ) ;
#1150 = DIRECTION ( 'NONE',  ( 0.000000000000000000, 1.000000000000000000, -0.000000000000000000 ) ) ;
#1151 = EDGE_CURVE ( 'NONE', #11003, #8866, #13588, .T. ) ;
#1152 = DIRECTION ( 'NONE',  ( 0.4528443260392607250, 0.8915896008669278450, 0.000000000000000000 ) ) ;
#1153 = CARTESIAN_POINT ( 'NONE',  ( -18.84164940403275423, 30.34709526170029648, 53.08392589000639816 ) ) ;
#1154 = DIRECTION ( 'NONE',  ( 0.000000000000000000, 0.000000000000000000, 1.000000000000000000 ) ) ;
#1155 = ORIENTED_EDGE ( 'NONE', *, *, #8188, .T. ) ;
#1156 = DIRECTION ( 'NONE',  ( 1.000000000000000000, 0.000000000000000000, 0.000000000000000000 ) ) ;
#1157 = CARTESIAN_POINT ( 'NONE',  ( -24.37001676333060018, -4.028726038184999858, 62.14999999999999858 ) ) ;
#1158 = DIRECTION ( 'NONE',  ( 1.000000000000000000, 0.000000000000000000, -0.000000000000000000 ) ) ;
#1159 = DIRECTION ( 'NONE',  ( 1.000000000000000000, 0.000000000000000000, 0.000000000000000000 ) ) ;
#1160 = VECTOR ( 'NONE', #6393, 1000.000000000000000 ) ;
#1161 = EDGE_CURVE ( 'NONE', #586, #956, #1938, .T. ) ;
#1162 = ORIENTED_EDGE ( 'NONE', *, *, #6210, .T. ) ;
#1163 = DIRECTION ( 'NONE',  ( 1.000000000000000000, 0.000000000000000000, 0.000000000000000000 ) ) ;
#1164 = VERTEX_POINT ( 'NONE', #3139 ) ;
#1165 = ORIENTED_EDGE ( 'NONE', *, *, #3279, .F. ) ;
#1167 = EDGE_CURVE ( 'NONE', #10572, #8384, #2508, .T. ) ;
#1166 = ORIENTED_EDGE ( 'NONE', *, *, #5935, .F. ) ;
#1168 = CARTESIAN_POINT ( 'NONE',  ( -18.05918829504999934, 10.97290950744599947, 62.14999999999999858 ) ) ;
#1169 = CIRCLE ( 'NONE', #4309, 10.74999999999999645 ) ;
#1170 = DIRECTION ( 'NONE',  ( 1.000000000000000000, 0.000000000000000000, 0.000000000000000000 ) ) ;
#1171 = DIRECTION ( 'NONE',  ( 1.000000000000000000, 0.000000000000000000, 0.000000000000000000 ) ) ;
#1172 = CARTESIAN_POINT ( 'NONE',  ( -18.05918829504999934, 10.97290950744599947, 68.84999999999999432 ) ) ;
#1173 = CARTESIAN_POINT ( 'NONE',  ( 83.82136590429891498, 114.1051029460540605, 10.00000000000000000 ) ) ;
#1174 = FACE_OUTER_BOUND ( 'NONE', #13468, .T. ) ;
#1175 = DIRECTION ( 'NONE',  ( -1.000000000000000000, 0.000000000000000000, 0.000000000000000000 ) ) ;
#1176 = ADVANCED_FACE ( 'NONE', ( #4173 ), #882, .F. ) ;
#1177 =( REPRESENTATION_RELATIONSHIP ('NONE','NONE', #11848, #5156 ) REPRESENTATION_RELATIONSHIP_WITH_TRANSFORMATION ( #13779 )SHAPE_REPRESENTATION_RELATIONSHIP( ) );
#1178 = CIRCLE ( 'NONE', #4978, 3.449999999999999734 ) ;
#1179 = VERTEX_POINT ( 'NONE', #3901 ) ;
#1180 = CARTESIAN_POINT ( 'NONE',  ( -16.38228052275427160, 30.29966228814565454, 53.43569657597039679 ) ) ;
#1181 = ORIENTED_EDGE ( 'NONE', *, *, #8350, .F. ) ;
#1182 = ADVANCED_FACE ( 'NONE', ( #9419, #12620 ), #5004, .T. ) ;
#1183 = DIRECTION ( 'NONE',  ( 0.000000000000000000, 0.000000000000000000, -1.000000000000000000 ) ) ;
#1184 = LINE ( 'NONE', #9716, #3596 ) ;
#1185 = LINE ( 'NONE', #9717, #10085 ) ;
#1186 = EDGE_LOOP ( 'NONE', ( #4778, #9164, #12277, #13400 ) ) ;
#1187 = CARTESIAN_POINT ( 'NONE',  ( 74.18094369249178044, 97.20665973629650125, 20.00000000000000000 ) ) ;
#1188 = LINE ( 'NONE', #6508, #1300 ) ;
#1189 = CIRCLE ( 'NONE', #3879, 8.395833332999997012 ) ;
#1190 = CARTESIAN_POINT ( 'NONE',  ( -1.627166789049998563, 19.18892026044596832, 63.36264408499989287 ) ) ;
#1191 = ADVANCED_FACE ( 'NONE', ( #8146 ), #3177, .T. ) ;
#1192 = LINE ( 'NONE', #12999, #11798 ) ;
#1193 = ORIENTED_EDGE ( 'NONE', *, *, #10839, .T. ) ;
#1194 = EDGE_LOOP ( 'NONE', ( #2877, #4120 ) ) ;
#1195 = DIRECTION ( 'NONE',  ( 0.000000000000000000, 0.000000000000000000, 1.000000000000000000 ) ) ;
#1196 = ORIENTED_EDGE ( 'NONE', *, *, #10990, .T. ) ;
#1197 = ORIENTED_EDGE ( 'NONE', *, *, #12093, .T. ) ;
#1198 = ORIENTED_EDGE ( 'NONE', *, *, #6040, .T. ) ;
#1199 = CYLINDRICAL_SURFACE ( 'NONE', #2450, 3.000000000000001332 ) ;
#1200 = DIRECTION ( 'NONE',  ( -1.000000000000000000, 0.000000000000000000, 0.000000000000000000 ) ) ;
#1201 = EDGE_LOOP ( 'NONE', ( #7692, #6041, #5461, #4296 ) ) ;
#1202 = DIRECTION ( 'NONE',  ( 0.000000000000000000, 0.000000000000000000, 1.000000000000000000 ) ) ;
#1203 = CARTESIAN_POINT ( 'NONE',  ( -17.20901794878084701, 26.95030579715291807, 56.11417500233394406 ) ) ;
#1204 = CARTESIAN_POINT ( 'NONE',  ( -35.05918829505000645, 27.97290950744599769, 64.35000000000000853 ) ) ;
#1205 = CARTESIAN_POINT ( 'NONE',  ( -18.05918829504999934, 10.97290950744599947, 30.59999999999999787 ) ) ;
#1206 = DIRECTION ( 'NONE',  ( 0.000000000000000000, 0.000000000000000000, 1.000000000000000000 ) ) ;
#1207 = EDGE_CURVE ( 'NONE', #755, #1411, #11435, .T. ) ;
#1208 = ORIENTED_EDGE ( 'NONE', *, *, #7558, .F. ) ;
#1209 = ORIENTED_EDGE ( 'NONE', *, *, #11415, .F. ) ;
#1210 = EDGE_LOOP ( 'NONE', ( #7018, #3341, #4736, #1690 ) ) ;
#1211 = CYLINDRICAL_SURFACE ( 'NONE', #7038, 12.00000000000000355 ) ;
#1212 = VERTEX_POINT ( 'NONE', #7285 ) ;
#1213 = DIRECTION ( 'NONE',  ( 0.000000000000000000, 0.000000000000000000, -1.000000000000000000 ) ) ;
#1214 = DIRECTION ( 'NONE',  ( 1.000000000000000000, 0.000000000000000000, -0.000000000000000000 ) ) ;
#1215 = DIRECTION ( 'NONE',  ( 1.000000000000000000, 0.000000000000000000, 0.000000000000000000 ) ) ;
#1216 = AXIS2_PLACEMENT_3D ( 'NONE', #1473, #7960, #11057 ) ;
#1217 = CARTESIAN_POINT ( 'NONE',  ( -18.74037715811554961, 30.35031926759491938, 53.06094751610090299 ) ) ;
#1218 = CARTESIAN_POINT ( 'NONE',  ( -39.30918829504999934, 27.97290950744599769, 64.35000000000000853 ) ) ;
#1219 = VERTEX_POINT ( 'NONE', #5070 ) ;
#1220 = DIRECTION ( 'NONE',  ( 0.000000000000000000, 0.000000000000000000, -1.000000000000000000 ) ) ;
#1221 = DIRECTION ( 'NONE',  ( 0.000000000000000000, 0.000000000000000000, 1.000000000000000000 ) ) ;
#1222 = CARTESIAN_POINT ( 'NONE',  ( -8.500000000000000000, 2.499999999999999556, -65.00000000000000000 ) ) ;
#1223 = CARTESIAN_POINT ( 'NONE',  ( 113.0903281124166710, 100.8715034839261762, 10.00000000000000000 ) ) ;
#1224 = SHAPE_REPRESENTATION_RELATIONSHIP ( 'NONE' , 'NONE' ,  #5062, #3759 ) ;
#1225 = EDGE_CURVE ( 'NONE', #4495, #721, #6178, .T. ) ;
#1226 = AXIS2_PLACEMENT_3D ( 'NONE', #13677, #3850, #13600 ) ;
#1227 = EDGE_CURVE ( 'NONE', #1958, #10203, #10982, .T. ) ;
#1228 = ORIENTED_EDGE ( 'NONE', *, *, #13497, .F. ) ;
#1229 = CARTESIAN_POINT ( 'NONE',  ( 50.63563590245420443, 103.9054980190242361, 22.75000000000000000 ) ) ;
#1230 = VERTEX_POINT ( 'NONE', #9272 ) ;
#1231 = ORIENTED_EDGE ( 'NONE', *, *, #5670, .T. ) ;
#1232 = DIRECTION ( 'NONE',  ( 0.4528443260392606695, 0.8915896008669279560, 0.000000000000000000 ) ) ;
#1233 = ORIENTED_EDGE ( 'NONE', *, *, #10224, .T. ) ;
#1234 = DIRECTION ( 'NONE',  ( 0.000000000000000000, 0.000000000000000000, -1.000000000000000000 ) ) ;
#1235 = CARTESIAN_POINT ( 'NONE',  ( 76.11748380738829667, 82.61803701715820125, 0.000000000000000000 ) ) ;
#1236 = LINE ( 'NONE', #3086, #12541 ) ;
#1237 = DIRECTION ( 'NONE',  ( -0.000000000000000000, 1.000000000000000000, -0.000000000000000000 ) ) ;
#1238 = LINE ( 'NONE', #12982, #4262 ) ;
#1239 = AXIS2_PLACEMENT_3D ( 'NONE', #13784, #5466, #12756 ) ;
#1240 = CARTESIAN_POINT ( 'NONE',  ( -18.05918829504999934, 10.97290950744599947, 58.54999999999999716 ) ) ;
#1241 = DIRECTION ( 'NONE',  ( 0.000000000000000000, 0.000000000000000000, -1.000000000000000000 ) ) ;
#1242 = ORIENTED_EDGE ( 'NONE', *, *, #6372, .T. ) ;
#1244 = EDGE_CURVE ( 'NONE', #11891, #1905, #6044, .T. ) ;
#1243 = UNCERTAINTY_MEASURE_WITH_UNIT (LENGTH_MEASURE( 1.000000000000000082E-05 ), #3583, 'distance_accuracy_value', 'NONE');
#1245 = ORIENTED_EDGE ( 'NONE', *, *, #8673, .T. ) ;
#1246 = VECTOR ( 'NONE', #11216, 1000.000000000000000 ) ;
#1247 = CARTESIAN_POINT ( 'NONE',  ( -15.75124634074425956, 30.24535125669912716, 53.87933641254778649 ) ) ;
#1248 = LINE ( 'NONE', #7515, #9967 ) ;
#1249 = EDGE_CURVE ( 'NONE', #12867, #1551, #4039, .T. ) ;
#1250 = CARTESIAN_POINT ( 'NONE',  ( -40.05918829504999934, -14.02709049255400053, 0.000000000000000000 ) ) ;
#1251 = DIRECTION ( 'NONE',  ( 0.000000000000000000, 0.000000000000000000, 1.000000000000000000 ) ) ;
#1252 = ORIENTED_EDGE ( 'NONE', *, *, #4145, .T. ) ;
#1253 = CARTESIAN_POINT ( 'NONE',  ( -12.69835982676941910, -4.028726038184999858, 62.14999999999999858 ) ) ;
#1254 = DIRECTION ( 'NONE',  ( 0.000000000000000000, 0.000000000000000000, -1.000000000000000000 ) ) ;
#1255 = AXIS2_PLACEMENT_3D ( 'NONE', #10138, #9994, #12087 ) ;
#1256 = CARTESIAN_POINT ( 'NONE',  ( 44.63563590245420443, 108.9054980190242503, 23.00000000000000000 ) ) ;
#1257 = EDGE_CURVE ( 'NONE', #1798, #10620, #10323, .T. ) ;
#1258 = ORIENTED_EDGE ( 'NONE', *, *, #10990, .F. ) ;
#1259 = ORIENTED_EDGE ( 'NONE', *, *, #7216, .F. ) ;
#1260 = ORIENTED_EDGE ( 'NONE', *, *, #10582, .F. ) ;
#1261 = VERTEX_POINT ( 'NONE', #7222 ) ;
#1262 = PLANE ( 'NONE',  #1009 ) ;
#1263 = VERTEX_POINT ( 'NONE', #7089 ) ;
#1264 = VERTEX_POINT ( 'NONE', #11367 ) ;
#1265 = ORIENTED_EDGE ( 'NONE', *, *, #12420, .T. ) ;
#1266 = VECTOR ( 'NONE', #6258, 1000.000000000000000 ) ;
#1267 = ADVANCED_FACE ( 'NONE', ( #9479 ), #1874, .T. ) ;
#1268 = DIRECTION ( 'NONE',  ( -0.000000000000000000, -0.000000000000000000, -1.000000000000000000 ) ) ;
#1269 = CARTESIAN_POINT ( 'NONE',  ( -28.87730642030694739, 29.81324547859995278, 83.57661607529820458 ) ) ;
#1270 = VERTEX_POINT ( 'NONE', #10383 ) ;
#1271 = CARTESIAN_POINT ( 'NONE',  ( 68.49370948373500312, 75.03908161011133870, 20.00000000000000000 ) ) ;
#1272 = LINE ( 'NONE', #2426, #4966 ) ;
#1273 = CARTESIAN_POINT ( 'NONE',  ( -23.42001676333060090, -4.028726038184999858, 62.14999999999999858 ) ) ;
#1274 = CARTESIAN_POINT ( 'NONE',  ( -18.88016301897669891, 16.91647750172969822, 64.85000000000000853 ) ) ;
#1275 = CARTESIAN_POINT ( 'NONE',  ( -18.05918829504999934, 10.97290950744599947, 62.14999999999999858 ) ) ;
#1276 = VECTOR ( 'NONE', #1860, 1000.000000000000000 ) ;
#1277 = ORIENTED_EDGE ( 'NONE', *, *, #10649, .F. ) ;
#1278 = COLOUR_RGB ( '', 0.08235294, 0.09019608, 0.10196078) ;
#1279 = VERTEX_POINT ( 'NONE', #13724 ) ;
#1280 = ORIENTED_EDGE ( 'NONE', *, *, #369, .F. ) ;
#1281 = VERTEX_POINT ( 'NONE', #9338 ) ;
#1282 = EDGE_CURVE ( 'NONE', #6154, #1279, #5373, .T. ) ;
#1283 = FACE_OUTER_BOUND ( 'NONE', #1055, .T. ) ;
#1284 = CIRCLE ( 'NONE', #7510, 6.299999999999998046 ) ;
#1285 = DIRECTION ( 'NONE',  ( 1.000000000000000000, 0.000000000000000000, 0.000000000000000000 ) ) ;
#1286 = EDGE_CURVE ( 'NONE', #9471, #9880, #10745, .T. ) ;
#1287 = CONICAL_SURFACE ( 'NONE', #5299, 16.95000000000000284, 0.7853981633974433940 ) ;
#1288 = DIRECTION ( 'NONE',  ( 0.000000000000000000, 0.000000000000000000, 1.000000000000000000 ) ) ;
#1289 = SURFACE_STYLE_USAGE ( .BOTH. , #6335 ) ;
#1290 = AXIS2_PLACEMENT_3D ( 'NONE', #10171, #9189, #2921 ) ;
#1291 = CARTESIAN_POINT ( 'NONE',  ( -19.57774717906803374, 30.31058478656889932, 53.35224432894259650 ) ) ;
#1292 = CARTESIAN_POINT ( 'NONE',  ( -2.059188295050000228, 10.97290950744599947, 7.250000000000000000 ) ) ;
#1293 = ORIENTED_EDGE ( 'NONE', *, *, #4670, .T. ) ;
#1294 = DIRECTION ( 'NONE',  ( 0.000000000000000000, 1.000000000000000000, 0.000000000000000000 ) ) ;
#1295 = DIRECTION ( 'NONE',  ( -1.000000000000000000, 0.000000000000000000, 0.000000000000000000 ) ) ;
#1296 = CARTESIAN_POINT ( 'NONE',  ( -15.41280400920135030, 7.973467857469549891, 27.30000000000000071 ) ) ;
#1297 = AXIS2_PLACEMENT_3D ( 'NONE', #13466, #11306, #1730 ) ;
#1298 = AXIS2_PLACEMENT_3D ( 'NONE', #9090, #13349, #2770 ) ;
#1299 = VECTOR ( 'NONE', #10129, 1000.000000000000000 ) ;
#1300 = VECTOR ( 'NONE', #8327, 1000.000000000000000 ) ;
#1301 = VERTEX_POINT ( 'NONE', #2227 ) ;
#1302 = EDGE_LOOP ( 'NONE', ( #10862, #1884 ) ) ;
#1303 = FACE_OUTER_BOUND ( 'NONE', #3883, .T. ) ;
#1304 = ORIENTED_EDGE ( 'NONE', *, *, #7232, .F. ) ;
#1305 = DIRECTION ( 'NONE',  ( 1.000000000000000000, 0.000000000000000000, 0.000000000000000000 ) ) ;
#1306 = LINE ( 'NONE', #2243, #817 ) ;
#1307 = FACE_OUTER_BOUND ( 'NONE', #9354, .T. ) ;
#1308 = DIRECTION ( 'NONE',  ( -1.000000000000000000, 0.000000000000000000, 0.000000000000000000 ) ) ;
#1309 = FACE_BOUND ( 'NONE', #7385, .T. ) ;
#1310 = EDGE_CURVE ( 'NONE', #135, #7821, #13435, .T. ) ;
#1311 = VECTOR ( 'NONE', #10141, 1000.000000000000000 ) ;
#1312 = AXIS2_PLACEMENT_3D ( 'NONE', #2805, #7025, #13669 ) ;
#1313 = CARTESIAN_POINT ( 'NONE',  ( -14.75120793773922045, 7.223607444975439940, 68.84999999999999432 ) ) ;
#1314 = ADVANCED_FACE ( 'NONE', ( #1019 ), #4448, .F. ) ;
#1315 = CARTESIAN_POINT ( 'NONE',  ( -18.05918829504999934, 10.97290950744599947, 56.84999999999999432 ) ) ;
#1316 = CIRCLE ( 'NONE', #4639, 3.449999999999999734 ) ;
#1317 = CARTESIAN_POINT ( 'NONE',  ( 0.000000000000000000, 0.000000000000000000, -43.00000000000000000 ) ) ;
#1318 = PLANE ( 'NONE',  #4202 ) ;
#1319 = ADVANCED_FACE ( 'NONE', ( #1086 ), #3472, .T. ) ;
#1320 = VECTOR ( 'NONE', #4212, 1000.000000000000000 ) ;
#1321 = CARTESIAN_POINT ( 'NONE',  ( -15.59876235566975744, 30.22970645086915198, 54.01720515842198012 ) ) ;
#1322 = VECTOR ( 'NONE', #5683, 1000.000000000000000 ) ;
#1323 = ORIENTED_EDGE ( 'NONE', *, *, #6995, .T. ) ;
#1324 = DIRECTION ( 'NONE',  ( 0.000000000000000000, 0.000000000000000000, 1.000000000000000000 ) ) ;
#1325 = DIRECTION ( 'NONE',  ( 0.000000000000000000, 1.000000000000000000, 0.000000000000000000 ) ) ;
#1326 = DIRECTION ( 'NONE',  ( 0.000000000000000000, 0.000000000000000000, -1.000000000000000000 ) ) ;
#1327 = ORIENTED_EDGE ( 'NONE', *, *, #11562, .T. ) ;
#1328 = DIRECTION ( 'NONE',  ( 0.000000000000000000, 0.000000000000000000, 1.000000000000000000 ) ) ;
#1329 = EDGE_CURVE ( 'NONE', #11446, #5675, #3215, .T. ) ;
#1330 = DIRECTION ( 'NONE',  ( 4.866859854469739928E-30, 2.732534507816520408E-15, 1.000000000000000000 ) ) ;
#1331 = ADVANCED_FACE ( 'NONE', ( #8274 ), #6161, .F. ) ;
#1332 = LINE ( 'NONE', #429, #5353 ) ;
#1333 = AXIS2_PLACEMENT_3D ( 'NONE', #2821, #5923, #8031 ) ;
#1334 = VECTOR ( 'NONE', #1010, 1000.000000000000000 ) ;
#1335 = ORIENTED_EDGE ( 'NONE', *, *, #6857, .T. ) ;
#1336 = ORIENTED_EDGE ( 'NONE', *, *, #1950, .F. ) ;
#1337 = ORIENTED_EDGE ( 'NONE', *, *, #10076, .F. ) ;
#1338 = DIRECTION ( 'NONE',  ( 0.6615960714621569316, -0.7498604124941123938, 0.000000000000000000 ) ) ;
#1339 = EDGE_LOOP ( 'NONE', ( #5946, #3463 ) ) ;
#1340 = ORIENTED_EDGE ( 'NONE', *, *, #10711, .F. ) ;
#1341 = AXIS2_PLACEMENT_3D ( 'NONE', #3898, #12351, #2799 ) ;
#1342 = ORIENTED_EDGE ( 'NONE', *, *, #10202, .T. ) ;
#1343 = VECTOR ( 'NONE', #1033, 999.9999999999998863 ) ;
#1344 = CONICAL_SURFACE ( 'NONE', #11169, 6.145833333000000565, 0.7853981633974503884 ) ;
#1345 = VECTOR ( 'NONE', #10978, 1000.000000000000000 ) ;
#1346 = LINE ( 'NONE', #8753, #7979 ) ;
#1347 = DIRECTION ( 'NONE',  ( 1.000000000000000000, 0.000000000000000000, 0.000000000000000000 ) ) ;
#1348 = EDGE_CURVE ( 'NONE', #12241, #3252, #9630, .T. ) ;
#1349 = FACE_OUTER_BOUND ( 'NONE', #5034, .T. ) ;
#1350 = FACE_OUTER_BOUND ( 'NONE', #10782, .T. ) ;
#1351 = CARTESIAN_POINT ( 'NONE',  ( -34.78181777225609750, 10.00028003023991907, 62.14999999999999858 ) ) ;
#1352 = LINE ( 'NONE', #13083, #12495 ) ;
#1353 = EDGE_CURVE ( 'NONE', #12408, #9471, #4156, .T. ) ;
#1354 = AXIS2_PLACEMENT_3D ( 'NONE', #12587, #4972, #11466 ) ;
#1355 = CIRCLE ( 'NONE', #10736, 17.00000000000000355 ) ;
#1356 = EDGE_LOOP ( 'NONE', ( #10786, #1413, #10050, #4133 ) ) ;
#1357 = ORIENTED_EDGE ( 'NONE', *, *, #11759, .T. ) ;
#1358 = ORIENTED_EDGE ( 'NONE', *, *, #9793, .F. ) ;
#1359 = ORIENTED_EDGE ( 'NONE', *, *, #2598, .T. ) ;
#1360 = DIRECTION ( 'NONE',  ( 0.000000000000000000, 0.000000000000000000, -1.000000000000000000 ) ) ;
#1361 = ORIENTED_EDGE ( 'NONE', *, *, #9651, .T. ) ;
#1362 = DIRECTION ( 'NONE',  ( -0.000000000000000000, 1.000000000000000000, -0.000000000000000000 ) ) ;
#1363 = ORIENTED_EDGE ( 'NONE', *, *, #662, .F. ) ;
#1364 = CARTESIAN_POINT ( 'NONE',  ( -18.05918829504999934, 10.97290950744599947, 11.50000000000000000 ) ) ;
#1365 = ADVANCED_FACE ( 'NONE', ( #655 ), #13575, .T. ) ;
#1366 = CARTESIAN_POINT ( 'NONE',  ( -21.77521107841160131, 30.06124217889628270, 58.40862893704163383 ) ) ;
#1367 = AXIS2_PLACEMENT_3D ( 'NONE', #5789, #6709, #8951 ) ;
#1368 = VECTOR ( 'NONE', #4300, 1000.000000000000000 ) ;
#1369 = ORIENTED_EDGE ( 'NONE', *, *, #155, .T. ) ;
#1370 = DIRECTION ( 'NONE',  ( 0.000000000000000000, 0.000000000000000000, 1.000000000000000000 ) ) ;
#1371 = CIRCLE ( 'NONE', #8739, 1.999999999999996669 ) ;
#1372 = CARTESIAN_POINT ( 'NONE',  ( -9.663354962050000552, 10.97290950744599947, 60.75000000000000000 ) ) ;
#1373 = CARTESIAN_POINT ( 'NONE',  ( 3.500000000000001776, 2.499999999999999556, 0.000000000000000000 ) ) ;
#1374 = CARTESIAN_POINT ( 'NONE',  ( -16.55918829504999579, 28.64232754551664684, 57.35000000000000142 ) ) ;
#1375 = EDGE_CURVE ( 'NONE', #8213, #9649, #487, .T. ) ;
#1376 = AXIS2_PLACEMENT_3D ( 'NONE', #4675, #11938, #2530 ) ;
#1377 = CIRCLE ( 'NONE', #930, 17.00000000000000355 ) ;
#1378 = ORIENTED_EDGE ( 'NONE', *, *, #1864, .T. ) ;
#1379 = ORIENTED_EDGE ( 'NONE', *, *, #5655, .F. ) ;
#1380 = DIRECTION ( 'NONE',  ( -1.000000000000000000, -2.529805069132845816E-16, 0.000000000000000000 ) ) ;
#1381 = LINE ( 'NONE', #5632, #3349 ) ;
#1382 = ORIENTED_EDGE ( 'NONE', *, *, #4879, .F. ) ;
#1383 = DIRECTION ( 'NONE',  ( 0.000000000000000000, -0.000000000000000000, -1.000000000000000000 ) ) ;
#1384 = DIRECTION ( 'NONE',  ( -0.000000000000000000, 1.000000000000000000, -0.000000000000000000 ) ) ;
#1385 = CARTESIAN_POINT ( 'NONE',  ( 7.500000000000000000, -0.5000000000000017764, -65.00000000000000000 ) ) ;
#1386 = DIRECTION ( 'NONE',  ( -0.000000000000000000, -0.000000000000000000, 1.000000000000000000 ) ) ;
#1387 = DIRECTION ( 'NONE',  ( 1.000000000000000000, 0.000000000000000000, 0.000000000000000000 ) ) ;
#1388 = LINE ( 'NONE', #342, #7140 ) ;
#1389 = CIRCLE ( 'NONE', #3641, 8.395833332999998788 ) ;
#1390 = DIRECTION ( 'NONE',  ( 1.000000000000000000, -8.410780489584519664E-16, 0.000000000000000000 ) ) ;
#1391 = DIRECTION ( 'NONE',  ( 0.000000000000000000, 1.000000000000000000, 0.000000000000000000 ) ) ;
#1392 = UNCERTAINTY_MEASURE_WITH_UNIT (LENGTH_MEASURE( 1.000000000000000082E-05 ), #1947, 'distance_accuracy_value', 'NONE');
#1393 = VERTEX_POINT ( 'NONE', #4923 ) ;
#1394 = EDGE_CURVE ( 'NONE', #7753, #7807, #8288, .T. ) ;
#1395 = VECTOR ( 'NONE', #3256, 1000.000000000000000 ) ;
#1396 = ORIENTED_EDGE ( 'NONE', *, *, #8194, .T. ) ;
#1397 = DIRECTION ( 'NONE',  ( 1.000000000000000000, 0.000000000000000000, 0.000000000000000000 ) ) ;
#1398 = ORIENTED_EDGE ( 'NONE', *, *, #11335, .T. ) ;
#1399 = CARTESIAN_POINT ( 'NONE',  ( -1.059188295049996231, 27.97290950744599769, 0.000000000000000000 ) ) ;
#1400 = CARTESIAN_POINT ( 'NONE',  ( -18.05918829504999934, 10.97290950744599947, 67.84999999999999432 ) ) ;
#1401 = FACE_OUTER_BOUND ( 'NONE', #4521, .T. ) ;
#1402 = LINE ( 'NONE', #11048, #7524 ) ;
#1403 =( BOUNDED_CURVE ( )  B_SPLINE_CURVE ( 3, ( #5809, #3725, #7972, #9944 ),
 .UNSPECIFIED., .F., .F. ) 
 B_SPLINE_CURVE_WITH_KNOTS ( ( 4, 4 ),
 ( 0.06314145699999899886, 0.9368585429999889413 ),
 .UNSPECIFIED. ) 
 CURVE ( )  GEOMETRIC_REPRESENTATION_ITEM ( )  RATIONAL_B_SPLINE_CURVE ( ( 0.9565783021659940433, 0.7697947703959779897, 0.7697947703959749921, 0.9565783021659860497 ) ) 
 REPRESENTATION_ITEM ( '' )  );
#1404 = FACE_OUTER_BOUND ( 'NONE', #8374, .T. ) ;
#1405 = DIRECTION ( 'NONE',  ( 2.612535355386759959E-17, 0.000000000000000000, 1.000000000000000000 ) ) ;
#1406 = AXIS2_PLACEMENT_3D ( 'NONE', #7837, #5605, #6651 ) ;
#1407 = EDGE_CURVE ( 'NONE', #8384, #9884, #13503, .T. ) ;
#1408 = ORIENTED_EDGE ( 'NONE', *, *, #6290, .T. ) ;
#1409 = EDGE_LOOP ( 'NONE', ( #8506, #3866, #11058, #3386 ) ) ;
#1410 = EDGE_CURVE ( 'NONE', #10847, #759, #5593, .T. ) ;
#1411 = VERTEX_POINT ( 'NONE', #3949 ) ;
#1412 = CARTESIAN_POINT ( 'NONE',  ( -34.25918829536686872, 2.872909506853352557, 63.35000000001154774 ) ) ;
#1413 = ORIENTED_EDGE ( 'NONE', *, *, #11360, .F. ) ;
#1414 = ORIENTED_EDGE ( 'NONE', *, *, #8081, .T. ) ;
#1415 = CIRCLE ( 'NONE', #9457, 7.150000000000001243 ) ;
#1416 = ORIENTED_EDGE ( 'NONE', *, *, #599, .T. ) ;
#1417 = ORIENTED_EDGE ( 'NONE', *, *, #9988, .F. ) ;
#1418 = CARTESIAN_POINT ( 'NONE',  ( -18.05918829504999934, 10.97290950744599947, 60.85000000000000142 ) ) ;
#1419 = DIRECTION ( 'NONE',  ( -0.000000000000000000, -0.000000000000000000, 1.000000000000000000 ) ) ;
#1420 = VERTEX_POINT ( 'NONE', #793 ) ;
#1421 = DIRECTION ( 'NONE',  ( 0.000000000000000000, 0.000000000000000000, 1.000000000000000000 ) ) ;
#1422 = LINE ( 'NONE', #152, #10118 ) ;
#1423 = CARTESIAN_POINT ( 'NONE',  ( -1.059188295049996231, -6.027090492554000534, 64.85000000000000853 ) ) ;
#1424 = CARTESIAN_POINT ( 'NONE',  ( -4.599650328638321461, 0.000000000000000000, -5.878124499050807472 ) ) ;
#1425 = EDGE_LOOP ( 'NONE', ( #8670, #4151, #1327, #8418 ) ) ;
#1426 = ADVANCED_FACE ( 'NONE', ( #235 ), #7590, .F. ) ;
#1427 = EDGE_LOOP ( 'NONE', ( #893, #4786, #13084, #12703 ) ) ;
#1428 = CARTESIAN_POINT ( 'NONE',  ( -27.49999999999998934, 9.000000000000000000, 29.99999999999999645 ) ) ;
#1429 = ORIENTED_EDGE ( 'NONE', *, *, #4536, .F. ) ;
#1430 = ORIENTED_EDGE ( 'NONE', *, *, #10166, .F. ) ;
#1431 = FACE_OUTER_BOUND ( 'NONE', #8321, .T. ) ;
#1432 = EDGE_CURVE ( 'NONE', #5796, #2636, #4422, .T. ) ;
#1433 = CARTESIAN_POINT ( 'NONE',  ( -20.58544311336878962, 30.22252884699266673, 60.61712719099885760 ) ) ;
#1434 = ORIENTED_EDGE ( 'NONE', *, *, #13277, .F. ) ;
#1435 = CARTESIAN_POINT ( 'NONE',  ( -35.05918829505000645, -6.027090492554000534, 83.57661607529820458 ) ) ;
#1436 = CARTESIAN_POINT ( 'NONE',  ( 16.04064420431708982, 4.500000000000000000, 11.30758658292212893 ) ) ;
#1437 = PLANE ( 'NONE',  #8954 ) ;
#1438 = FACE_BOUND ( 'NONE', #6006, .T. ) ;
#1439 = EDGE_CURVE ( 'NONE', #3793, #7909, #4068, .T. ) ;
#1440 = VERTEX_POINT ( 'NONE', #7338 ) ;
#1441 = AXIS2_PLACEMENT_3D ( 'NONE', #11116, #13337, #1544 ) ;
#1442 = LINE ( 'NONE', #471, #4155 ) ;
#1443 = APPLICATION_CONTEXT ( 'automotive_design' ) ;
#1444 = DIRECTION ( 'NONE',  ( -0.000000000000000000, -0.000000000000000000, 1.000000000000000000 ) ) ;
#1445 = LINE ( 'NONE', #8925, #6698 ) ;
#1446 = LINE ( 'NONE', #8851, #5059 ) ;
#1447 = EDGE_CURVE ( 'NONE', #6660, #9517, #3124, .T. ) ;
#1448 = FACE_OUTER_BOUND ( 'NONE', #13325, .T. ) ;
#1449 = CARTESIAN_POINT ( 'NONE',  ( 42.63563590245419732, 111.0390816101113387, 0.7500000000000006661 ) ) ;
#1450 = CARTESIAN_POINT ( 'NONE',  ( 112.1804561881462945, 112.2890816101113387, 0.7500000000000006661 ) ) ;
#1451 = DIRECTION ( 'NONE',  ( 0.000000000000000000, 0.000000000000000000, -1.000000000000000000 ) ) ;
#1452 = DIRECTION ( 'NONE',  ( 0.000000000000000000, 0.000000000000000000, 1.000000000000000000 ) ) ;
#1453 = CARTESIAN_POINT ( 'NONE',  ( -30.30918829504999934, -6.027090492554000534, 64.85000000000000853 ) ) ;
#1454 = DIRECTION ( 'NONE',  ( 1.000000000000000000, 0.000000000000000000, 0.000000000000000000 ) ) ;
#1455 = CARTESIAN_POINT ( 'NONE',  ( -18.05918829504999934, 10.97290950744599947, 7.250000000000000000 ) ) ;
#1456 = VECTOR ( 'NONE', #11799, 1000.000000000000000 ) ;
#1457 = ORIENTED_EDGE ( 'NONE', *, *, #10898, .F. ) ;
#1458 = ORIENTED_EDGE ( 'NONE', *, *, #1257, .T. ) ;
#1459 = FACE_OUTER_BOUND ( 'NONE', #9173, .T. ) ;
#1460 = ORIENTED_EDGE ( 'NONE', *, *, #70, .T. ) ;
#1461 = VECTOR ( 'NONE', #2767, 1000.000000000000000 ) ;
#1462 = EDGE_LOOP ( 'NONE', ( #7418, #7086, #12382, #7454 ) ) ;
#1463 = DIRECTION ( 'NONE',  ( 0.000000000000000000, 0.000000000000000000, 1.000000000000000000 ) ) ;
#1464 = VECTOR ( 'NONE', #2656, 1000.000000000000000 ) ;
#1465 = EDGE_CURVE ( 'NONE', #13804, #13429, #12960, .T. ) ;
#1466 = FACE_OUTER_BOUND ( 'NONE', #7959, .T. ) ;
#1467 = DIRECTION ( 'NONE',  ( 0.000000000000000000, -1.000000000000000000, 0.000000000000000000 ) ) ;
#1468 = FACE_BOUND ( 'NONE', #12423, .T. ) ;
#1469 = LINE ( 'NONE', #12164, #4699 ) ;
#1470 = FACE_BOUND ( 'NONE', #9238, .T. ) ;
#1471 = AXIS2_PLACEMENT_3D ( 'NONE', #9039, #1639, #8322 ) ;
#1472 = ORIENTED_EDGE ( 'NONE', *, *, #10632, .T. ) ;
#1473 = CARTESIAN_POINT ( 'NONE',  ( -18.05918829504999934, 21.47290950744600124, 57.35000000000000142 ) ) ;
#1474 = EDGE_LOOP ( 'NONE', ( #536, #2988, #9030, #307 ) ) ;
#1475 = ORIENTED_EDGE ( 'NONE', *, *, #8339, .T. ) ;
#1476 = ORIENTED_EDGE ( 'NONE', *, *, #13544, .T. ) ;
#1477 = ORIENTED_EDGE ( 'NONE', *, *, #865, .T. ) ;
#1478 = DIRECTION ( 'NONE',  ( 0.000000000000000000, 0.000000000000000000, 1.000000000000000000 ) ) ;
#1479 = ORIENTED_EDGE ( 'NONE', *, *, #9694, .T. ) ;
#1480 = CARTESIAN_POINT ( 'NONE',  ( -18.05918829504999934, 10.97290950744599947, 118.8499999999999943 ) ) ;
#1481 = ORIENTED_EDGE ( 'NONE', *, *, #577, .T. ) ;
#1482 = AXIS2_PLACEMENT_3D ( 'NONE', #5818, #8768, #4514 ) ;
#1483 = CARTESIAN_POINT ( 'NONE',  ( -24.37001676333060018, -4.028726038184999858, 62.14999999999999858 ) ) ;
#1484 = CARTESIAN_POINT ( 'NONE',  ( -16.85695709240152951, 26.92898083073637494, 56.44676063695975188 ) ) ;
#1485 = EDGE_CURVE ( 'NONE', #11380, #936, #11628, .T. ) ;
#1486 = CARTESIAN_POINT ( 'NONE',  ( -18.05918829504999934, 10.97290950744599947, 62.14999999999999858 ) ) ;
#1487 = EDGE_CURVE ( 'NONE', #11722, #6370, #1136, .T. ) ;
#1488 = EDGE_CURVE ( 'NONE', #10360, #2746, #8543, .T. ) ;
#1489 = ORIENTED_EDGE ( 'NONE', *, *, #11587, .T. ) ;
#1490 = AXIS2_PLACEMENT_3D ( 'NONE', #6835, #5787, #10070 ) ;
#1491 = VERTEX_POINT ( 'NONE', #5455 ) ;
#1492 = DIRECTION ( 'NONE',  ( -0.000000000000000000, -0.000000000000000000, 1.000000000000000000 ) ) ;
#1493 = EDGE_LOOP ( 'NONE', ( #9757, #11508, #6256, #13606 ) ) ;
#1494 = LINE ( 'NONE', #526, #7505 ) ;
#1495 = CARTESIAN_POINT ( 'NONE',  ( -20.84535740604768250, 30.19258199390759145, 60.33062495464709940 ) ) ;
#1496 = LINE ( 'NONE', #11920, #1629 ) ;
#1497 = DIRECTION ( 'NONE',  ( 0.3132098788326365124, -0.9496839325805429555, 0.000000000000000000 ) ) ;
#1498 = DIRECTION ( 'NONE',  ( 0.000000000000000000, 0.000000000000000000, 1.000000000000000000 ) ) ;
#1499 = CARTESIAN_POINT ( 'NONE',  ( -18.05918829504999934, 10.97290950744599947, 63.14999999999999858 ) ) ;
#1500 = EDGE_CURVE ( 'NONE', #6209, #7736, #4425, .T. ) ;
#1501 = COLOUR_RGB ( '', 0.72549020, 0.75294118, 0.79215686) ;
#1502 = CARTESIAN_POINT ( 'NONE',  ( 0.000000000000000000, 0.000000000000000000, 7.000000000000000000 ) ) ;
#1503 = ORIENTED_EDGE ( 'NONE', *, *, #3611, .F. ) ;
#1504 = ADVANCED_FACE ( 'NONE', ( #11829 ), #4229, .F. ) ;
#1505 = TOROIDAL_SURFACE ( 'NONE', #9776, 16.99999999999999645, 1.500000000000000000 ) ;
#1506 = ORIENTED_EDGE ( 'NONE', *, *, #489, .T. ) ;
#1507 = AXIS2_PLACEMENT_3D ( 'NONE', #3121, #3758, #2073 ) ;
#1508 = CARTESIAN_POINT ( 'NONE',  ( -18.05918829504999934, 10.97290950744599947, 31.09999999999999787 ) ) ;
#1509 = DIRECTION ( 'NONE',  ( 0.000000000000000000, 0.000000000000000000, 1.000000000000000000 ) ) ;
#1510 = DIRECTION ( 'NONE',  ( 0.8915896008669277339, -0.4528443260392608916, 0.000000000000000000 ) ) ;
#1511 = FACE_OUTER_BOUND ( 'NONE', #6643, .T. ) ;
#1512 = CARTESIAN_POINT ( 'NONE',  ( -18.05918829504999934, 10.97290950744599947, 64.85000000000000853 ) ) ;
#1513 = CARTESIAN_POINT ( 'NONE',  ( -10.38347696868452097, 26.08535324214045303, 60.85000000000000142 ) ) ;
#1514 = EDGE_CURVE ( 'NONE', #8485, #3005, #5525, .T. ) ;
#1515 = DIRECTION ( 'NONE',  ( -0.000000000000000000, -0.000000000000000000, 1.000000000000000000 ) ) ;
#1516 = CARTESIAN_POINT ( 'NONE',  ( -9.759188295050000406, 10.97290950744599947, 63.14999999999999858 ) ) ;
#1517 = CARTESIAN_POINT ( 'NONE',  ( -14.95720466168106100, 17.08029827338444662, 61.25000000000000000 ) ) ;
#1518 = DIRECTION ( 'NONE',  ( -0.000000000000000000, -0.000000000000000000, -1.000000000000000000 ) ) ;
#1519 = EDGE_CURVE ( 'NONE', #5154, #11963, #6379, .T. ) ;
#1520 = DIRECTION ( 'NONE',  ( 0.000000000000000000, 0.000000000000000000, 1.000000000000000000 ) ) ;
#1521 = FACE_OUTER_BOUND ( 'NONE', #2833, .T. ) ;
#1522 = AXIS2_PLACEMENT_3D ( 'NONE', #13541, #9363, #3089 ) ;
#1523 = AXIS2_PLACEMENT_3D ( 'NONE', #5451, #4423, #2834 ) ;
#1524 = CIRCLE ( 'NONE', #1746, 34.69999999999999574 ) ;
#1525 = CIRCLE ( 'NONE', #7516, 3.000000000000000888 ) ;
#1526 = ADVANCED_FACE ( 'NONE', ( #9672, #3311 ), #9524, .T. ) ;
#1527 = UNCERTAINTY_MEASURE_WITH_UNIT (LENGTH_MEASURE( 1.000000000000000082E-05 ), #2265, 'distance_accuracy_value', 'NONE');
#1528 = EDGE_CURVE ( 'NONE', #2555, #12583, #256, .T. ) ;
#1529 = EDGE_LOOP ( 'NONE', ( #7431, #11443 ) ) ;
#1530 = VERTEX_POINT ( 'NONE', #7616 ) ;
#1531 = MECHANICAL_DESIGN_GEOMETRIC_PRESENTATION_REPRESENTATION (  '', ( #9796 ), #10238 ) ;
#1532 = AXIS2_PLACEMENT_3D ( 'NONE', #10626, #4480, #1046 ) ;
#1533 = AXIS2_PLACEMENT_3D ( 'NONE', #12415, #2868, #7092 ) ;
#1534 = VERTEX_POINT ( 'NONE', #11903 ) ;
#1535 = CARTESIAN_POINT ( 'NONE',  ( -1.059188295049996231, 10.97290950744599947, 57.35000000000000142 ) ) ;
#1536 = AXIS2_PLACEMENT_3D ( 'NONE', #515, #10094, #7614 ) ;
#1537 = CYLINDRICAL_SURFACE ( 'NONE', #10957, 0.7500000000000000000 ) ;
#1538 = CARTESIAN_POINT ( 'NONE',  ( -18.05918829504999934, 28.64232754551664684, 57.35000000000000142 ) ) ;
#1539 = DIRECTION ( 'NONE',  ( 0.4528443260392610026, 0.8915896008669278450, 0.000000000000000000 ) ) ;
#1540 = EDGE_CURVE ( 'NONE', #10854, #13546, #9597, .T. ) ;
#1541 = DIRECTION ( 'NONE',  ( 0.000000000000000000, 0.000000000000000000, 1.000000000000000000 ) ) ;
#1542 = FACE_OUTER_BOUND ( 'NONE', #12537, .T. ) ;
#1543 = ADVANCED_FACE ( 'NONE', ( #9812 ), #3195, .T. ) ;
#1544 = DIRECTION ( 'NONE',  ( 1.000000000000000000, 0.000000000000000000, 0.000000000000000000 ) ) ;
#1545 = AXIS2_PLACEMENT_3D ( 'NONE', #9327, #13508, #10178 ) ;
#1546 = EDGE_CURVE ( 'NONE', #10428, #6071, #1377, .T. ) ;
#1547 = AXIS2_PLACEMENT_3D ( 'NONE', #5114, #6150, #10357 ) ;
#1548 = ORIENTED_EDGE ( 'NONE', *, *, #5160, .F. ) ;
#1549 = ORIENTED_EDGE ( 'NONE', *, *, #12646, .F. ) ;
#1550 = CARTESIAN_POINT ( 'NONE',  ( -17.37799943181128626, 30.35031926759487675, 61.63905248387093394 ) ) ;
#1551 = VERTEX_POINT ( 'NONE', #3458 ) ;
#1552 = VERTEX_POINT ( 'NONE', #7683 ) ;
#1553 = EDGE_LOOP ( 'NONE', ( #3942, #7911, #7578, #6630, #552, #7539, #7897, #7173, #3995, #4191, #5278, #1888, #2472, #13515, #9187, #10950, #53, #11982, #4644, #8269, #4358 ) ) ;
#1554 = FACE_OUTER_BOUND ( 'NONE', #3019, .T. ) ;
#1555 = DIRECTION ( 'NONE',  ( -1.000000000000000000, 0.000000000000000000, 0.000000000000000000 ) ) ;
#1556 = DIRECTION ( 'NONE',  ( -0.000000000000000000, -0.000000000000000000, -1.000000000000000000 ) ) ;
#1557 = ORIENTED_EDGE ( 'NONE', *, *, #892, .T. ) ;
#1558 = DIRECTION ( 'NONE',  ( 0.000000000000000000, 0.000000000000000000, 1.000000000000000000 ) ) ;
#1559 = CIRCLE ( 'NONE', #4687, 17.00000000000000355 ) ;
#1560 = FACE_OUTER_BOUND ( 'NONE', #1201, .T. ) ;
#1561 = VECTOR ( 'NONE', #10811, 1000.000000000000000 ) ;
#1562 = CYLINDRICAL_SURFACE ( 'NONE', #11812, 8.250000000000001776 ) ;
#1563 = CARTESIAN_POINT ( 'NONE',  ( -11.06274345774342116, 24.74796884084004844, 57.35000000000000142 ) ) ;
#1564 = AXIS2_PLACEMENT_3D ( 'NONE', #13614, #12313, #696 ) ;
#1565 = VECTOR ( 'NONE', #5716, 1000.000000000000000 ) ;
#1566 = EDGE_CURVE ( 'NONE', #1261, #6644, #5611, .T. ) ;
#1567 = VERTEX_POINT ( 'NONE', #7763 ) ;
#1568 = CARTESIAN_POINT ( 'NONE',  ( 101.4499059006094512, 83.97306027416853169, 10.00000000000000000 ) ) ;
#1569 = VERTEX_POINT ( 'NONE', #6930 ) ;
#1570 = CARTESIAN_POINT ( 'NONE',  ( -21.31400196563854266, 30.13112197624766964, 59.63668312139478900 ) ) ;
#1571 = FACE_OUTER_BOUND ( 'NONE', #13452, .T. ) ;
#1572 = FACE_OUTER_BOUND ( 'NONE', #2832, .T. ) ;
#1573 = CARTESIAN_POINT ( 'NONE',  ( 140.6356359024541973, 89.90549801902423610, 23.00000000000000000 ) ) ;
#1574 = DIRECTION ( 'NONE',  ( -1.000000000000000000, 0.000000000000000000, 0.000000000000000000 ) ) ;
#1575 = CYLINDRICAL_SURFACE ( 'NONE', #8023, 4.749999999999997335 ) ;
#1576 = CIRCLE ( 'NONE', #12727, 4.750000000000000000 ) ;
#1577 = AXIS2_PLACEMENT_3D ( 'NONE', #2529, #11157, #11297 ) ;
#1578 = DIRECTION ( 'NONE',  ( 1.000000000000000000, 0.000000000000000000, 0.000000000000000000 ) ) ;
#1579 = AXIS2_PLACEMENT_3D ( 'NONE', #3244, #2063, #927 ) ;
#1580 = AXIS2_PLACEMENT_3D ( 'NONE', #8151, #5909, #3640 ) ;
#1581 = ORIENTED_EDGE ( 'NONE', *, *, #12580, .F. ) ;
#1582 = ADVANCED_FACE ( 'NONE', ( #8819 ), #11065, .F. ) ;
#1583 = DIRECTION ( 'NONE',  ( 0.000000000000000000, 0.000000000000000000, 1.000000000000000000 ) ) ;
#1584 = AXIS2_PLACEMENT_3D ( 'NONE', #12805, #10716, #1202 ) ;
#1585 = CARTESIAN_POINT ( 'NONE',  ( 116.7775623211734342, 85.03908161011133870, 0.7500000000000006661 ) ) ;
#1586 = VECTOR ( 'NONE', #9342, 1000.000000000000000 ) ;
#1587 = VERTEX_POINT ( 'NONE', #8893 ) ;
#1588 = CYLINDRICAL_SURFACE ( 'NONE', #1341, 8.395833332999997012 ) ;
#1589 = CARTESIAN_POINT ( 'NONE',  ( -11.75918829505000041, 10.97290950744599947, 61.86500000000000199 ) ) ;
#1590 = FACE_OUTER_BOUND ( 'NONE', #6386, .T. ) ;
#1591 = CARTESIAN_POINT ( 'NONE',  ( -38.38077571930825371, 22.44393519180574970, 17.25000000000000000 ) ) ;
#1592 = DIRECTION ( 'NONE',  ( 1.000000000000000000, 0.000000000000000000, 0.000000000000000000 ) ) ;
#1593 = DIRECTION ( 'NONE',  ( 0.000000000000000000, -1.000000000000000000, 0.000000000000000000 ) ) ;
#1594 = CARTESIAN_POINT ( 'NONE',  ( -24.03999999999999915, 0.000000000000000000, 7.000000000000000000 ) ) ;
#1595 = CARTESIAN_POINT ( 'NONE',  ( -12.69835982676941910, -4.028726038184999858, 63.45000000000000284 ) ) ;
#1596 = CARTESIAN_POINT ( 'NONE',  ( 50.63563590245420443, 108.9054980190242503, 22.75000000000000000 ) ) ;
#1597 = DIRECTION ( 'NONE',  ( 0.000000000000000000, 0.000000000000000000, -1.000000000000000000 ) ) ;
#1598 = EDGE_CURVE ( 'NONE', #318, #1219, #8736, .T. ) ;
#1599 = AXIS2_PLACEMENT_3D ( 'NONE', #2786, #1786, #7208 ) ;
#1600 = AXIS2_PLACEMENT_3D ( 'NONE', #6949, #10176, #10041 ) ;
#1601 = ORIENTED_EDGE ( 'NONE', *, *, #4222, .T. ) ;
#1602 = EDGE_CURVE ( 'NONE', #11352, #997, #3845, .T. ) ;
#1603 = ORIENTED_EDGE ( 'NONE', *, *, #8859, .F. ) ;
#1604 = VERTEX_POINT ( 'NONE', #5732 ) ;
#1605 = DIRECTION ( 'NONE',  ( -1.000000000000000000, 0.000000000000000000, 0.000000000000000000 ) ) ;
#1606 = ORIENTED_EDGE ( 'NONE', *, *, #13740, .T. ) ;
#1607 = FACE_OUTER_BOUND ( 'NONE', #10170, .T. ) ;
#1608 = COLOUR_RGB ( '', 0.08235294, 0.09019608, 0.10196078) ;
#1609 = DIRECTION ( 'NONE',  ( 1.000000000000000000, 0.000000000000000000, 0.000000000000000000 ) ) ;
#1610 = CARTESIAN_POINT ( 'NONE',  ( -1.059188295049996231, 27.97290950744599769, 64.35000000000000853 ) ) ;
#1611 = EDGE_CURVE ( 'NONE', #8462, #755, #266, .T. ) ;
#1612 = CARTESIAN_POINT ( 'NONE',  ( 68.49370948373500312, 123.0390816101113245, 0.000000000000000000 ) ) ;
#1613 = DIRECTION ( 'NONE',  ( 1.000000000000000000, 0.000000000000000000, -0.000000000000000000 ) ) ;
#1614 = DIRECTION ( 'NONE',  ( 0.000000000000000000, 1.000000000000000000, -0.000000000000000000 ) ) ;
#1615 = VECTOR ( 'NONE', #5971, 1000.000000000000000 ) ;
#1616 = ADVANCED_FACE ( 'NONE', ( #1628 ), #10158, .F. ) ;
#1617 = EDGE_LOOP ( 'NONE', ( #1773, #7606, #6309, #2503 ) ) ;
#1618 = DIRECTION ( 'NONE',  ( 0.000000000000000000, 0.000000000000000000, 1.000000000000000000 ) ) ;
#1619 = VECTOR ( 'NONE', #3466, 1000.000000000000000 ) ;
#1620 = ORIENTED_EDGE ( 'NONE', *, *, #9892, .T. ) ;
#1621 = ORIENTED_EDGE ( 'NONE', *, *, #1485, .F. ) ;
#1622 = CARTESIAN_POINT ( 'NONE',  ( 6.940811704950004213, 32.97290950744599769, 0.000000000000000000 ) ) ;
#1623 = ORIENTED_EDGE ( 'NONE', *, *, #4075, .T. ) ;
#1624 = CARTESIAN_POINT ( 'NONE',  ( -18.05918829504999934, 10.97290950744599947, 63.45000000000000284 ) ) ;
#1625 = DIRECTION ( 'NONE',  ( -0.000000000000000000, 0.000000000000000000, -1.000000000000000000 ) ) ;
#1626 = DIRECTION ( 'NONE',  ( -0.000000000000000000, 1.000000000000000000, -0.000000000000000000 ) ) ;
#1627 = ADVANCED_FACE ( 'NONE', ( #3602 ), #13288, .F. ) ;
#1628 = FACE_OUTER_BOUND ( 'NONE', #9221, .T. ) ;
#1629 = VECTOR ( 'NONE', #6805, 1000.000000000000000 ) ;
#1630 = DIRECTION ( 'NONE',  ( 1.000000000000000000, 0.000000000000000000, 0.000000000000000000 ) ) ;
#1631 = CARTESIAN_POINT ( 'NONE',  ( -18.05918829504999934, 10.97290950744599947, 10.00000000000000000 ) ) ;
#1632 = CARTESIAN_POINT ( 'NONE',  ( 140.3856359024541973, 104.1554980190242361, 23.00000000000000000 ) ) ;
#1633 = VERTEX_POINT ( 'NONE', #6732 ) ;
#1634 = ORIENTED_EDGE ( 'NONE', *, *, #10598, .F. ) ;
#1635 = AXIS2_PLACEMENT_3D ( 'NONE', #6619, #924, #3431 ) ;
#1636 = VERTEX_POINT ( 'NONE', #7836 ) ;
#1637 = ORIENTED_EDGE ( 'NONE', *, *, #12185, .T. ) ;
#1638 = ORIENTED_EDGE ( 'NONE', *, *, #13674, .T. ) ;
#1639 = DIRECTION ( 'NONE',  ( 0.000000000000000000, 0.000000000000000000, 1.000000000000000000 ) ) ;
#1640 = CARTESIAN_POINT ( 'NONE',  ( -16.55918829504999579, 27.90660372932210009, 57.35000000000000142 ) ) ;
#1641 = CARTESIAN_POINT ( 'NONE',  ( -20.70149429739183944, 30.20956267044833865, 60.49614159523773793 ) ) ;
#1642 = DIRECTION ( 'NONE',  ( 0.000000000000000000, -1.000000000000000000, 1.672022627447524796E-15 ) ) ;
#1643 = DIRECTION ( 'NONE',  ( -2.267612386897784912E-16, 1.000000000000000000, 0.000000000000000000 ) ) ;
#1644 = DIRECTION ( 'NONE',  ( -0.000000000000000000, -1.000000000000000000, -0.000000000000000000 ) ) ;
#1645 = AXIS2_PLACEMENT_3D ( 'NONE', #5776, #3696, #1454 ) ;
#1646 = CARTESIAN_POINT ( 'NONE',  ( -18.05918829504999934, 14.81548537210212046, 5.250000000000000000 ) ) ;
#1647 = DIRECTION ( 'NONE',  ( 1.000000000000000000, 0.000000000000000000, 1.224646799147353207E-16 ) ) ;
#1648 = EDGE_CURVE ( 'NONE', #4985, #10572, #10929, .T. ) ;
#1649 = EDGE_LOOP ( 'NONE', ( #12050, #2259, #5190, #4837 ) ) ;
#1650 = LINE ( 'NONE', #5897, #9500 ) ;
#1651 = CARTESIAN_POINT ( 'NONE',  ( 134.6356359024541973, 89.90549801902423610, 22.75000000000000000 ) ) ;
#1652 = EDGE_LOOP ( 'NONE', ( #10510, #6611, #2690, #10999 ) ) ;
#1653 = CARTESIAN_POINT ( 'NONE',  ( -30.48673169511680214, 10.97290950744599947, 17.25000000000000000 ) ) ;
#1654 = CARTESIAN_POINT ( 'NONE',  ( -18.05918829504999934, 10.97290950744599947, 23.90000000000000213 ) ) ;
#1655 = DIRECTION ( 'NONE',  ( -1.000000000000000000, 0.000000000000000000, 0.000000000000000000 ) ) ;
#1656 = CARTESIAN_POINT ( 'NONE',  ( 116.7775623211734342, 113.0390816101113387, 0.7500000000000006661 ) ) ;
#1657 = LINE ( 'NONE', #12482, #1615 ) ;
#1658 = ORIENTED_EDGE ( 'NONE', *, *, #1074, .F. ) ;
#1659 = LINE ( 'NONE', #8662, #11567 ) ;
#1660 = LINE ( 'NONE', #7289, #5099 ) ;
#1661 = DIRECTION ( 'NONE',  ( -0.9496839325805428444, -0.3132098788326364569, 0.000000000000000000 ) ) ;
#1662 = DIRECTION ( 'NONE',  ( 0.000000000000000000, 0.000000000000000000, 1.000000000000000000 ) ) ;
#1663 = CARTESIAN_POINT ( 'NONE',  ( -7.241070169793059286, -7.867426463707969830, 17.25000000000000000 ) ) ;
#1664 = EDGE_CURVE ( 'NONE', #2189, #3894, #5167, .T. ) ;
#1665 = ADVANCED_FACE ( 'NONE', ( #7903 ), #5879, .T. ) ;
#1666 = UNCERTAINTY_MEASURE_WITH_UNIT (LENGTH_MEASURE( 1.000000000000000082E-05 ), #5163, 'distance_accuracy_value', 'NONE');
#1667 = VERTEX_POINT ( 'NONE', #11132 ) ;
#1668 = ORIENTED_EDGE ( 'NONE', *, *, #2700, .T. ) ;
#1669 = CYLINDRICAL_SURFACE ( 'NONE', #2379, 24.04163056034261459 ) ;
#1670 = EDGE_LOOP ( 'NONE', ( #10777, #2517, #12810, #4417 ) ) ;
#1671 = ORIENTED_EDGE ( 'NONE', *, *, #1519, .F. ) ;
#1672 = CARTESIAN_POINT ( 'NONE',  ( 16.45469220996245241, 1.832421873814834345, 7.000000000000000000 ) ) ;
#1673 = LINE ( 'NONE', #4757, #6249 ) ;
#1674 =( NAMED_UNIT ( * ) PLANE_ANGLE_UNIT ( ) SI_UNIT ( $, .RADIAN. ) );
#1675 = CARTESIAN_POINT ( 'NONE',  ( 0.000000000000000000, 8.500000000000000000, 0.000000000000000000 ) ) ;
#1676 = AXIS2_PLACEMENT_3D ( 'NONE', #13416, #5794, #8171 ) ;
#1677 = CARTESIAN_POINT ( 'NONE',  ( -18.05918829504999223, 19.18892026044601096, 63.36264408500002787 ) ) ;
#1678 = DIRECTION ( 'NONE',  ( 0.000000000000000000, 0.000000000000000000, -1.000000000000000000 ) ) ;
#1679 = EDGE_CURVE ( 'NONE', #13687, #10707, #1403, .T. ) ;
#1680 = DIRECTION ( 'NONE',  ( 0.000000000000000000, 0.000000000000000000, -1.000000000000000000 ) ) ;
#1681 = ADVANCED_FACE ( 'NONE', ( #1349 ), #3523, .F. ) ;
#1682 = ORIENTED_EDGE ( 'NONE', *, *, #3550, .F. ) ;
#1683 = EDGE_CURVE ( 'NONE', #9990, #11639, #2703, .T. ) ;
#1684 = VECTOR ( 'NONE', #5986, 1000.000000000000000 ) ;
#1685 = CARTESIAN_POINT ( 'NONE',  ( -17.32805791519659522, 30.34876749365187720, 61.62799931076499860 ) ) ;
#1686 = ORIENTED_EDGE ( 'NONE', *, *, #688, .T. ) ;
#1687 = VERTEX_POINT ( 'NONE', #4567 ) ;
#1688 = CARTESIAN_POINT ( 'NONE',  ( -1.336558817843898073, 10.00028003023991907, 63.45000000000000284 ) ) ;
#1689 = FACE_BOUND ( 'NONE', #9516, .T. ) ;
#1690 = ORIENTED_EDGE ( 'NONE', *, *, #8139, .T. ) ;
#1691 = DIRECTION ( 'NONE',  ( -1.000000000000000000, 0.000000000000000000, 0.000000000000000000 ) ) ;
#1692 = FACE_OUTER_BOUND ( 'NONE', #8193, .T. ) ;
#1693 = CARTESIAN_POINT ( 'NONE',  ( 18.45469220996244886, 1.832421873814834123, 7.000000000000000000 ) ) ;
#1694 = DIRECTION ( 'NONE',  ( -0.000000000000000000, 1.000000000000000000, -0.000000000000000000 ) ) ;
#1695 = CARTESIAN_POINT ( 'NONE',  ( -18.25896549665364432, 27.97289716965712358, 58.84983448222843805 ) ) ;
#1696 = EDGE_CURVE ( 'NONE', #9008, #10592, #4507, .T. ) ;
#1697 = CARTESIAN_POINT ( 'NONE',  ( 140.6356359024541973, 103.9054980190242361, 22.89644660940672694 ) ) ;
#1698 = EDGE_CURVE ( 'NONE', #6077, #12394, #12449, .T. ) ;
#1699 = ORIENTED_EDGE ( 'NONE', *, *, #4145, .F. ) ;
#1700 = ADVANCED_FACE ( 'NONE', ( #11407 ), #710, .T. ) ;
#1701 = ORIENTED_EDGE ( 'NONE', *, *, #1854, .T. ) ;
#1702 = ORIENTED_EDGE ( 'NONE', *, *, #11140, .T. ) ;
#1703 = AXIS2_PLACEMENT_3D ( 'NONE', #3465, #2364, #248 ) ;
#1704 = DIRECTION ( 'NONE',  ( 0.000000000000000000, 0.000000000000000000, -1.000000000000000000 ) ) ;
#1705 = CARTESIAN_POINT ( 'NONE',  ( -20.33293068681281923, 30.24873049275584691, 60.84977818423778473 ) ) ;
#1706 = DIRECTION ( 'NONE',  ( 0.000000000000000000, 0.000000000000000000, 1.000000000000000000 ) ) ;
#1707 = CARTESIAN_POINT ( 'NONE',  ( -18.05918829504999934, 10.97290950744599947, 60.75000000000000000 ) ) ;
#1708 = DIRECTION ( 'NONE',  ( 0.4528443260392608916, 0.8915896008669279560, 0.000000000000000000 ) ) ;
#1709 = CARTESIAN_POINT ( 'NONE',  ( -0.04028432657539327000, 4.500000000000000000, 18.54539866546729243 ) ) ;
#1710 = DIRECTION ( 'NONE',  ( 1.224646799147353207E-16, 0.000000000000000000, -1.000000000000000000 ) ) ;
#1711 = EDGE_LOOP ( 'NONE', ( #4221, #4676, #1668, #12719 ) ) ;
#1712 = EDGE_LOOP ( 'NONE', ( #6233, #12262, #6482, #5448 ) ) ;
#1713 = AXIS2_PLACEMENT_3D ( 'NONE', #9012, #13263, #11589 ) ;
#1714 = EDGE_CURVE ( 'NONE', #12649, #2384, #8715, .T. ) ;
#1715 = EDGE_LOOP ( 'NONE', ( #8381, #3310, #9397, #11626 ) ) ;
#1716 = CARTESIAN_POINT ( 'NONE',  ( -18.05918829504999934, 10.97290950744599947, 12.50000000000000000 ) ) ;
#1717 = ORIENTED_EDGE ( 'NONE', *, *, #3656, .T. ) ;
#1718 = CIRCLE ( 'NONE', #158, 3.000000000000002665 ) ;
#1719 = ORIENTED_EDGE ( 'NONE', *, *, #11656, .T. ) ;
#1720 = DIRECTION ( 'NONE',  ( 0.4528443260392608916, 0.8915896008669277339, 0.000000000000000000 ) ) ;
#1721 = CARTESIAN_POINT ( 'NONE',  ( -5.809188295050001116, -6.027090492554000534, 64.85000000000000853 ) ) ;
#1722 = AXIS2_PLACEMENT_3D ( 'NONE', #1168, #2319, #12976 ) ;
#1723 = DIRECTION ( 'NONE',  ( 1.000000000000000000, 0.000000000000000000, 0.000000000000000000 ) ) ;
#1724 = CARTESIAN_POINT ( 'NONE',  ( -35.55918829505000645, 10.97290950744599947, 64.85000000000000853 ) ) ;
#1725 = CARTESIAN_POINT ( 'NONE',  ( -22.68187722381259519, 13.56225431454274677, 68.55150892931679607 ) ) ;
#1726 = CARTESIAN_POINT ( 'NONE',  ( 134.6356359024541973, 108.9054980190242503, 20.00000000000000000 ) ) ;
#1727 = CARTESIAN_POINT ( 'NONE',  ( 116.7775623211734342, 123.0390816101113245, 19.25000000000000000 ) ) ;
#1728 = DIRECTION ( 'NONE',  ( 1.000000000000000000, 0.000000000000000000, 0.000000000000000000 ) ) ;
#1729 = DIRECTION ( 'NONE',  ( 0.000000000000000000, 0.000000000000000000, 1.000000000000000000 ) ) ;
#1730 = DIRECTION ( 'NONE',  ( 1.000000000000000000, 0.000000000000000000, 0.000000000000000000 ) ) ;
#1731 = AXIS2_PLACEMENT_3D ( 'NONE', #5256, #12746, #13270 ) ;
#1732 = ADVANCED_FACE ( 'NONE', ( #2908 ), #10420, .T. ) ;
#1733 = CIRCLE ( 'NONE', #8449, 6.000000000000002665 ) ;
#1734 = AXIS2_PLACEMENT_3D ( 'NONE', #5337, #1018, #3331 ) ;
#1735 = VERTEX_POINT ( 'NONE', #3797 ) ;
#1736 = CARTESIAN_POINT ( 'NONE',  ( 44.73918929304747394, 90.00905140961751272, 23.00000000000000000 ) ) ;
#1737 = ORIENTED_EDGE ( 'NONE', *, *, #8744, .F. ) ;
#1738 = EDGE_CURVE ( 'NONE', #5595, #11930, #4484, .T. ) ;
#1739 = ADVANCED_FACE ( 'NONE', ( #1985, #7256 ), #8123, .F. ) ;
#1740 = ORIENTED_EDGE ( 'NONE', *, *, #8433, .T. ) ;
#1741 = CARTESIAN_POINT ( 'NONE',  ( -20.80749866017044880, 15.21600409713747304, 68.79477705781098962 ) ) ;
#1742 = DIRECTION ( 'NONE',  ( 0.4528443260392608916, 0.8915896008669277339, 0.000000000000000000 ) ) ;
#1743 = VECTOR ( 'NONE', #2328, 1000.000000000000000 ) ;
#1744 = CARTESIAN_POINT ( 'NONE',  ( -18.05918829504999934, 10.97290950744599947, 64.85000000000000853 ) ) ;
#1745 = AXIS2_PLACEMENT_3D ( 'NONE', #12207, #274, #3424 ) ;
#1746 = AXIS2_PLACEMENT_3D ( 'NONE', #5773, #483, #3965 ) ;
#1747 = DIRECTION ( 'NONE',  ( 0.000000000000000000, 0.000000000000000000, 1.000000000000000000 ) ) ;
#1748 = AXIS2_PLACEMENT_3D ( 'NONE', #1918, #10241, #7069 ) ;
#1749 = CARTESIAN_POINT ( 'NONE',  ( -18.05918829504999934, 2.673908674445999889, 63.13003331699999876 ) ) ;
#1750 = CARTESIAN_POINT ( 'NONE',  ( -25.86749127492459976, 30.80589556422609832, 5.250000000000000000 ) ) ;
#1751 = DIRECTION ( 'NONE',  ( 0.000000000000000000, 1.000000000000000000, 0.000000000000000000 ) ) ;
#1752 = ADVANCED_BREP_SHAPE_REPRESENTATION ( '', ( #8946, #6434 ), #2891 ) ;
#1753 = EDGE_CURVE ( 'NONE', #13237, #7790, #1807, .T. ) ;
#1754 = VECTOR ( 'NONE', #10980, 1000.000000000000000 ) ;
#1755 = VECTOR ( 'NONE', #2060, 1000.000000000000000 ) ;
#1756 = CIRCLE ( 'NONE', #10916, 16.66282263685194920 ) ;
#1757 = ORIENTED_EDGE ( 'NONE', *, *, #3815, .F. ) ;
#1758 = AXIS2_PLACEMENT_3D ( 'NONE', #13253, #7796, #482 ) ;
#1759 = ORIENTED_EDGE ( 'NONE', *, *, #13685, .F. ) ;
#1760 = CARTESIAN_POINT ( 'NONE',  ( -15.65696070512129268, 30.23571877985226664, 60.73654365824928192 ) ) ;
#1761 = ADVANCED_FACE ( 'NONE', ( #12525 ), #10355, .F. ) ;
#1762 = ORIENTED_EDGE ( 'NONE', *, *, #7451, .T. ) ;
#1763 = SURFACE_STYLE_FILL_AREA ( #11400 ) ;
#1764 = CARTESIAN_POINT ( 'NONE',  ( 12.00000000000000000, -2.499999999999999556, -65.00000000000000000 ) ) ;
#1765 = ORIENTED_EDGE ( 'NONE', *, *, #8460, .F. ) ;
#1766 = ORIENTED_EDGE ( 'NONE', *, *, #3092, .F. ) ;
#1767 = DIRECTION ( 'NONE',  ( 1.000000000000000000, 0.000000000000000000, 0.000000000000000000 ) ) ;
#1768 = CARTESIAN_POINT ( 'NONE',  ( 134.6356359024541973, 103.9054980190242361, 23.00000000000000000 ) ) ;
#1769 = EDGE_LOOP ( 'NONE', ( #13762, #13610, #6302, #4328 ) ) ;
#1770 = EDGE_CURVE ( 'NONE', #1905, #5559, #11471, .T. ) ;
#1771 = CARTESIAN_POINT ( 'NONE',  ( 44.63563590245421864, 85.03908161011133870, 0.7500000000000000000 ) ) ;
#1772 = DIRECTION ( 'NONE',  ( -1.000000000000000000, 0.000000000000000000, 0.000000000000000000 ) ) ;
#1773 = ORIENTED_EDGE ( 'NONE', *, *, #61, .T. ) ;
#1774 = AXIS2_PLACEMENT_3D ( 'NONE', #9931, #558, #1539 ) ;
#1775 = DIRECTION ( 'NONE',  ( 0.000000000000000000, 0.000000000000000000, 1.000000000000000000 ) ) ;
#1776 = CIRCLE ( 'NONE', #2234, 1.999999999999991340 ) ;
#1777 = EDGE_CURVE ( 'NONE', #11822, #7821, #6148, .T. ) ;
#1778 = LINE ( 'NONE', #9313, #243 ) ;
#1779 =( BOUNDED_CURVE ( )  B_SPLINE_CURVE ( 3, ( #12956, #11769, #8621, #9542 ),
 .UNSPECIFIED., .F., .F. ) 
 B_SPLINE_CURVE_WITH_KNOTS ( ( 4, 4 ),
 ( 3.141592653589793116, 4.712388980384689674 ),
 .UNSPECIFIED. ) 
 CURVE ( )  GEOMETRIC_REPRESENTATION_ITEM ( )  RATIONAL_B_SPLINE_CURVE ( ( 1.000000000000000000, 0.8047378541243649375, 0.8047378541243649375, 1.000000000000000000 ) ) 
 REPRESENTATION_ITEM ( '' )  );
#1780 = EDGE_CURVE ( 'NONE', #11171, #1958, #578, .T. ) ;
#1781 = ORIENTED_EDGE ( 'NONE', *, *, #9253, .F. ) ;
#1782 = VECTOR ( 'NONE', #374, 1000.000000000000000 ) ;
#1783 = CONICAL_SURFACE ( 'NONE', #4021, 16.00000000000000000, 0.7853981633974476129 ) ;
#1784 = VERTEX_POINT ( 'NONE', #9246 ) ;
#1785 = CARTESIAN_POINT ( 'NONE',  ( -18.05918829504999934, 10.97290950744599947, 61.86500000000000199 ) ) ;
#1786 = DIRECTION ( 'NONE',  ( -0.000000000000000000, -0.000000000000000000, 1.000000000000000000 ) ) ;
#1787 = DIRECTION ( 'NONE',  ( 0.4528443260392608916, 0.8915896008669279560, 0.000000000000000000 ) ) ;
#1788 = LINE ( 'NONE', #5892, #3741 ) ;
#1789 = CARTESIAN_POINT ( 'NONE',  ( -10.78334210919089919, 29.19143287883919768, 64.85000000000000853 ) ) ;
#1790 = EDGE_CURVE ( 'NONE', #13129, #13550, #2981, .T. ) ;
#1791 = DIRECTION ( 'NONE',  ( -0.000000000000000000, 1.000000000000000000, -0.000000000000000000 ) ) ;
#1792 = APPLICATION_PROTOCOL_DEFINITION ( 'draft international standard', 'automotive_design', 1998, #8323 ) ;
#1793 = AXIS2_PLACEMENT_3D ( 'NONE', #5792, #9017, #13271 ) ;
#1794 = AXIS2_PLACEMENT_3D ( 'NONE', #7342, #5199, #7546 ) ;
#1795 = ADVANCED_FACE ( 'NONE', ( #11537 ), #10284, .T. ) ;
#1796 = CARTESIAN_POINT ( 'NONE',  ( 7.500000000000000000, -0.5000000000000017764, 0.000000000000000000 ) ) ;
#1797 = EDGE_LOOP ( 'NONE', ( #899, #4051 ) ) ;
#1798 = VERTEX_POINT ( 'NONE', #12593 ) ;
#1799 = CARTESIAN_POINT ( 'NONE',  ( -35.05918829505000645, 10.97290950744599947, 64.35000000000000853 ) ) ;
#1800 = CARTESIAN_POINT ( 'NONE',  ( -18.05918829504999934, 10.97290950744599947, 61.85000000000000142 ) ) ;
#1801 = DIRECTION ( 'NONE',  ( 0.000000000000000000, 0.000000000000000000, 1.000000000000000000 ) ) ;
#1802 = VECTOR ( 'NONE', #6818, 1000.000000000000000 ) ;
#1803 = AXIS2_PLACEMENT_3D ( 'NONE', #4818, #4693, #10276 ) ;
#1804 = VECTOR ( 'NONE', #4144, 1000.000000000000000 ) ;
#1805 = DIRECTION ( 'NONE',  ( -1.000000000000000000, 0.000000000000000000, 0.000000000000000000 ) ) ;
#1806 = CARTESIAN_POINT ( 'NONE',  ( 1.640811704950000172, -6.027090492554000534, 58.85000000000000142 ) ) ;
#1807 = CIRCLE ( 'NONE', #228, 2.700000000000000178 ) ;
#1808 = FACE_OUTER_BOUND ( 'NONE', #7399, .T. ) ;
#1809 = PLANE ( 'NONE',  #475 ) ;
#1810 = EDGE_CURVE ( 'NONE', #194, #5817, #3936, .T. ) ;
#1811 = DIRECTION ( 'NONE',  ( 0.000000000000000000, 0.000000000000000000, 1.000000000000000000 ) ) ;
#1812 = FACE_BOUND ( 'NONE', #8651, .T. ) ;
#1813 = UNCERTAINTY_MEASURE_WITH_UNIT (LENGTH_MEASURE( 1.000000000000000082E-05 ), #10879, 'distance_accuracy_value', 'NONE');
#1814 = AXIS2_PLACEMENT_3D ( 'NONE', #5408, #6257, #99 ) ;
#1815 = AXIS2_PLACEMENT_3D ( 'NONE', #2245, #11724, #9640 ) ;
#1816 = AXIS2_PLACEMENT_3D ( 'NONE', #11578, #12485, #7290 ) ;
#1817 = ORIENTED_EDGE ( 'NONE', *, *, #5404, .F. ) ;
#1818 = VERTEX_POINT ( 'NONE', #6996 ) ;
#1819 = EDGE_LOOP ( 'NONE', ( #6252, #4124, #2486, #10182 ) ) ;
#1820 = CARTESIAN_POINT ( 'NONE',  ( -20.70557258089865016, 13.97235115742243927, 27.30000000000000071 ) ) ;
#1821 = VERTEX_POINT ( 'NONE', #13352 ) ;
#1822 = VERTEX_POINT ( 'NONE', #11270 ) ;
#1823 = DIRECTION ( 'NONE',  ( 0.000000000000000000, 0.000000000000000000, 1.000000000000000000 ) ) ;
#1824 = CARTESIAN_POINT ( 'NONE',  ( -18.05918829504999934, 14.81548537210212046, 64.85000000000000853 ) ) ;
#1825 = DIRECTION ( 'NONE',  ( -0.3984948954980490621, 0.000000000000000000, 0.9171705502587831349 ) ) ;
#1826 = AXIS2_PLACEMENT_3D ( 'NONE', #8216, #3010, #12481 ) ;
#1827 = FACE_OUTER_BOUND ( 'NONE', #10780, .T. ) ;
#1828 = AXIS2_PLACEMENT_3D ( 'NONE', #3461, #7621, #11906 ) ;
#1829 = CARTESIAN_POINT ( 'NONE',  ( -1.059188295049996231, 27.97290950744599769, 64.85000000000000853 ) ) ;
#1830 = EDGE_CURVE ( 'NONE', #9038, #11639, #3153, .T. ) ;
#1831 = ORIENTED_EDGE ( 'NONE', *, *, #6135, .T. ) ;
#1832 = EDGE_LOOP ( 'NONE', ( #8526, #8359, #2040, #9188, #3719, #8864, #8867, #3023, #5613, #8596, #1757, #6530, #6187, #11312, #2638 ) ) ;
#1833 = CIRCLE ( 'NONE', #5609, 2.000000000000001776 ) ;
#1834 = VERTEX_POINT ( 'NONE', #643 ) ;
#1835 = CARTESIAN_POINT ( 'NONE',  ( -15.83721163932141529, 30.25376030684627082, 60.89272510006725980 ) ) ;
#1836 = ORIENTED_EDGE ( 'NONE', *, *, #1810, .T. ) ;
#1837 = CARTESIAN_POINT ( 'NONE',  ( 92.63563590245421153, 85.78908161011133870, 19.25000000000000000 ) ) ;
#1838 = CARTESIAN_POINT ( 'NONE',  ( -18.05918829504999934, 10.97290950744599947, 61.86500000000000199 ) ) ;
#1839 = ORIENTED_EDGE ( 'NONE', *, *, #7568, .F. ) ;
#1840 = DIRECTION ( 'NONE',  ( 0.000000000000000000, 0.000000000000000000, 1.000000000000000000 ) ) ;
#1841 = ORIENTED_EDGE ( 'NONE', *, *, #12911, .F. ) ;
#1842 = DIRECTION ( 'NONE',  ( 0.000000000000000000, 0.000000000000000000, 1.000000000000000000 ) ) ;
#1843 = FACE_OUTER_BOUND ( 'NONE', #10573, .T. ) ;
#1844 = DIRECTION ( 'NONE',  ( 0.000000000000000000, 0.000000000000000000, -1.000000000000000000 ) ) ;
#1845 = DIRECTION ( 'NONE',  ( 0.4528443260392610581, 0.8915896008669278450, 0.000000000000000000 ) ) ;
#1846 = AXIS2_PLACEMENT_3D ( 'NONE', #6539, #2228, #13666 ) ;
#1847 = EDGE_CURVE ( 'NONE', #8804, #5387, #1238, .T. ) ;
#1848 = VERTEX_POINT ( 'NONE', #13696 ) ;
#1849 = ORIENTED_EDGE ( 'NONE', *, *, #4848, .F. ) ;
#1850 = ORIENTED_EDGE ( 'NONE', *, *, #10144, .F. ) ;
#1851 = EDGE_LOOP ( 'NONE', ( #8904, #12789, #1012, #5990 ) ) ;
#1852 = VERTEX_POINT ( 'NONE', #9921 ) ;
#1853 = AXIS2_PLACEMENT_3D ( 'NONE', #12468, #5052, #2924 ) ;
#1854 = EDGE_CURVE ( 'NONE', #9534, #5483, #122, .T. ) ;
#1855 = EDGE_LOOP ( 'NONE', ( #9780, #9648, #6092, #7714 ) ) ;
#1856 = ORIENTED_EDGE ( 'NONE', *, *, #11943, .F. ) ;
#1857 = DIRECTION ( 'NONE',  ( 0.000000000000000000, 0.000000000000000000, -1.000000000000000000 ) ) ;
#1858 = CARTESIAN_POINT ( 'NONE',  ( -20.28967185382198224, 30.25294134169608995, 60.88576449748650532 ) ) ;
#1859 = CARTESIAN_POINT ( 'NONE',  ( -4.499999999999999112, -1.301042606982605321E-15, -65.00000000000000000 ) ) ;
#1860 = DIRECTION ( 'NONE',  ( 0.3202092937642119774, 0.6304490528084089052, 0.7071067811865507924 ) ) ;
#1861 = CARTESIAN_POINT ( 'NONE',  ( 44.63563590245420443, 94.90549801902425031, 22.75000000000000000 ) ) ;
#1862 = CYLINDRICAL_SURFACE ( 'NONE', #3130, 1.999999999999991340 ) ;
#1863 = SHAPE_DEFINITION_REPRESENTATION ( #8638, #2236 ) ;
#1864 = EDGE_CURVE ( 'NONE', #8825, #2555, #11613, .T. ) ;
#1865 = EDGE_CURVE ( 'NONE', #8537, #9462, #5639, .T. ) ;
#1866 = EDGE_CURVE ( 'NONE', #6343, #8303, #1388, .T. ) ;
#1867 = CARTESIAN_POINT ( 'NONE',  ( -2.059188295050000228, 10.97290950744599947, 64.85000000000000853 ) ) ;
#1868 = EDGE_CURVE ( 'NONE', #12210, #5647, #8268, .T. ) ;
#1869 = ORIENTED_EDGE ( 'NONE', *, *, #3418, .T. ) ;
#1870 = ORIENTED_EDGE ( 'NONE', *, *, #1865, .F. ) ;
#1871 = DIRECTION ( 'NONE',  ( 0.2000659497483225358, -2.450101249776580428E-17, 0.9797824328652262604 ) ) ;
#1872 = LINE ( 'NONE', #12556, #7490 ) ;
#1873 = CIRCLE ( 'NONE', #76, 23.49999999999999645 ) ;
#1874 = CYLINDRICAL_SURFACE ( 'NONE', #1826, 15.45000000000000462 ) ;
#1875 = CARTESIAN_POINT ( 'NONE',  ( -22.74060393451187423, 13.51044018961873938, 68.52518719986740336 ) ) ;
#1876 = ORIENTED_EDGE ( 'NONE', *, *, #11038, .F. ) ;
#1877 = DIRECTION ( 'NONE',  ( -0.000000000000000000, -1.000000000000000000, 0.000000000000000000 ) ) ;
#1878 = CARTESIAN_POINT ( 'NONE',  ( -6.000000000000000888, -12.00000000000000178, 0.000000000000000000 ) ) ;
#1879 = CARTESIAN_POINT ( 'NONE',  ( -16.40519811639460102, 9.098258476210720147, 53.85000000000000142 ) ) ;
#1880 = CARTESIAN_POINT ( 'NONE',  ( 134.6356359024541973, 103.9054980190242361, 22.75000000000000000 ) ) ;
#1881 = FACE_OUTER_BOUND ( 'NONE', #13106, .T. ) ;
#1882 = ORIENTED_EDGE ( 'NONE', *, *, #5382, .F. ) ;
#1883 = EDGE_CURVE ( 'NONE', #1954, #4388, #923, .T. ) ;
#1884 = ORIENTED_EDGE ( 'NONE', *, *, #10411, .T. ) ;
#1885 = ADVANCED_FACE ( 'NONE', ( #12077 ), #3808, .T. ) ;
#1886 = ORIENTED_EDGE ( 'NONE', *, *, #12222, .F. ) ;
#1887 = CARTESIAN_POINT ( 'NONE',  ( -18.05918829504999934, 21.47290950744600124, 57.35000000000000142 ) ) ;
#1888 = ORIENTED_EDGE ( 'NONE', *, *, #4118, .T. ) ;
#1889 = ORIENTED_EDGE ( 'NONE', *, *, #734, .T. ) ;
#1890 = CARTESIAN_POINT ( 'NONE',  ( -18.05918829504999934, 10.97290950744599947, 61.72253826518770836 ) ) ;
#1891 = CIRCLE ( 'NONE', #7214, 6.449999999999997513 ) ;
#1892 = FACE_OUTER_BOUND ( 'NONE', #6374, .T. ) ;
#1893 = CARTESIAN_POINT ( 'NONE',  ( 74.18094369249178044, 97.20665973629650125, 10.00000000000000000 ) ) ;
#1894 = CARTESIAN_POINT ( 'NONE',  ( 44.94629607423404849, 85.78908161011133870, 20.00000000000000000 ) ) ;
#1895 = DIRECTION ( 'NONE',  ( -1.000000000000000000, -0.000000000000000000, 0.000000000000000000 ) ) ;
#1896 = ORIENTED_EDGE ( 'NONE', *, *, #562, .F. ) ;
#1897 = EDGE_CURVE ( 'NONE', #7689, #4189, #7657, .T. ) ;
#1898 = CARTESIAN_POINT ( 'NONE',  ( -14.68608402389303613, 30.11415384993292221, 59.40884097298657451 ) ) ;
#1899 = EDGE_CURVE ( 'NONE', #1411, #2899, #10959, .T. ) ;
#1900 = ORIENTED_EDGE ( 'NONE', *, *, #12612, .F. ) ;
#1901 = ORIENTED_EDGE ( 'NONE', *, *, #4528, .F. ) ;
#1902 = CARTESIAN_POINT ( 'NONE',  ( 142.6356359024541973, 87.03908161011133870, 0.7500000000000000000 ) ) ;
#1903 = DIRECTION ( 'NONE',  ( 0.000000000000000000, 0.000000000000000000, -1.000000000000000000 ) ) ;
#1904 = DIRECTION ( 'NONE',  ( 0.000000000000000000, 0.000000000000000000, 1.000000000000000000 ) ) ;
#1905 = VERTEX_POINT ( 'NONE', #12659 ) ;
#1906 = DIRECTION ( 'NONE',  ( 0.000000000000000000, 0.000000000000000000, -1.000000000000000000 ) ) ;
#1907 = PLANE ( 'NONE',  #7309 ) ;
#1908 = DIRECTION ( 'NONE',  ( 1.000000000000000000, 0.000000000000000000, 0.000000000000000000 ) ) ;
#1909 = CARTESIAN_POINT ( 'NONE',  ( -30.80918829504999934, -6.027090492554000534, 58.85000000000000142 ) ) ;
#1910 = CARTESIAN_POINT ( 'NONE',  ( -35.05918829505000645, -6.027090492554000534, 17.25000000000000000 ) ) ;
#1911 = DIRECTION ( 'NONE',  ( -1.000000000000000000, 0.000000000000000000, 0.000000000000000000 ) ) ;
#1912 = AXIS2_PLACEMENT_3D ( 'NONE', #5352, #6403, #10673 ) ;
#1913 = ORIENTED_EDGE ( 'NONE', *, *, #7508, .F. ) ;
#1914 = ORIENTED_EDGE ( 'NONE', *, *, #5344, .T. ) ;
#1915 = EDGE_CURVE ( 'NONE', #1552, #3512, #11940, .T. ) ;
#1916 = ORIENTED_EDGE ( 'NONE', *, *, #1432, .T. ) ;
#1917 = EDGE_CURVE ( 'NONE', #3017, #10813, #3374, .T. ) ;
#1918 = CARTESIAN_POINT ( 'NONE',  ( -18.05918829504999934, 14.81548537210212046, 83.57661607529820458 ) ) ;
#1919 = AXIS2_PLACEMENT_3D ( 'NONE', #10965, #5557, #1380 ) ;
#1920 = CARTESIAN_POINT ( 'NONE',  ( -19.69645725958885762, 30.30251685228200031, 61.28626485309589356 ) ) ;
#1921 = ORIENTED_EDGE ( 'NONE', *, *, #10224, .F. ) ;
#1922 = CARTESIAN_POINT ( 'NONE',  ( 4.599650328638321461, 0.000000000000000000, 9.878124499050780827 ) ) ;
#1923 = ADVANCED_FACE ( 'NONE', ( #4142 ), #13390, .F. ) ;
#1924 = FACE_OUTER_BOUND ( 'NONE', #6017, .T. ) ;
#1925 = CARTESIAN_POINT ( 'NONE',  ( -18.05918829504999934, 10.97290950744599947, 57.35000000000000142 ) ) ;
#1926 = FACE_BOUND ( 'NONE', #3735, .T. ) ;
#1927 = DIRECTION ( 'NONE',  ( 1.000000000000000000, 0.000000000000000000, 0.000000000000000000 ) ) ;
#1928 = ORIENTED_EDGE ( 'NONE', *, *, #12110, .F. ) ;
#1929 = EDGE_LOOP ( 'NONE', ( #10797, #758, #11962, #439, #12567, #2606 ) ) ;
#1930 = AXIS2_PLACEMENT_3D ( 'NONE', #9743, #9681, #3265 ) ;
#1931 = DIRECTION ( 'NONE',  ( 0.4528443260392610581, 0.8915896008669278450, 0.000000000000000000 ) ) ;
#1932 = FACE_OUTER_BOUND ( 'NONE', #10506, .T. ) ;
#1933 = CIRCLE ( 'NONE', #3717, 1.999999999999994893 ) ;
#1934 = VERTEX_POINT ( 'NONE', #7327 ) ;
#1935 = DIRECTION ( 'NONE',  ( 0.000000000000000000, 0.000000000000000000, -1.000000000000000000 ) ) ;
#1936 = ADVANCED_FACE ( 'NONE', ( #278 ), #13049, .T. ) ;
#1937 = DIRECTION ( 'NONE',  ( 0.000000000000000000, 0.000000000000000000, -1.000000000000000000 ) ) ;
#1938 = LINE ( 'NONE', #13665, #7827 ) ;
#1939 = ORIENTED_EDGE ( 'NONE', *, *, #2072, .T. ) ;
#1940 = LINE ( 'NONE', #6111, #280 ) ;
#1941 = EDGE_LOOP ( 'NONE', ( #150, #11027, #10349, #12721 ) ) ;
#1942 = DIRECTION ( 'NONE',  ( 1.000000000000000000, 0.000000000000000000, 0.000000000000000000 ) ) ;
#1943 = DIRECTION ( 'NONE',  ( -0.000000000000000000, -0.000000000000000000, 1.000000000000000000 ) ) ;
#1944 = DIRECTION ( 'NONE',  ( 0.000000000000000000, 0.000000000000000000, 1.000000000000000000 ) ) ;
#1945 = VECTOR ( 'NONE', #5991, 1000.000000000000000 ) ;
#1946 = CARTESIAN_POINT ( 'NONE',  ( -25.64433075620760150, -3.961216307075045240, 58.54999999999999716 ) ) ;
#1947 =( LENGTH_UNIT ( ) NAMED_UNIT ( * ) SI_UNIT ( .MILLI., .METRE. ) );
#1948 = EDGE_LOOP ( 'NONE', ( #8762, #258 ) ) ;
#1949 = EDGE_CURVE ( 'NONE', #10148, #2653, #6694, .T. ) ;
#1950 = EDGE_CURVE ( 'NONE', #6107, #10154, #13176, .T. ) ;
#1951 = AXIS2_PLACEMENT_3D ( 'NONE', #11496, #10450, #3896 ) ;
#1952 = VERTEX_POINT ( 'NONE', #9453 ) ;
#1953 = AXIS2_PLACEMENT_3D ( 'NONE', #4110, #7283, #3007 ) ;
#1954 = VERTEX_POINT ( 'NONE', #6555 ) ;
#1955 = CARTESIAN_POINT ( 'NONE',  ( -13.40033457972183939, -4.525318844826149878, 62.14999999999999858 ) ) ;
#1956 = ORIENTED_EDGE ( 'NONE', *, *, #11434, .F. ) ;
#1957 = ORIENTED_EDGE ( 'NONE', *, *, #8761, .F. ) ;
#1958 = VERTEX_POINT ( 'NONE', #3353 ) ;
#1959 = ADVANCED_FACE ( 'NONE', ( #7586 ), #11874, .F. ) ;
#1960 = DIRECTION ( 'NONE',  ( 0.000000000000000000, 0.000000000000000000, 1.000000000000000000 ) ) ;
#1961 = DIRECTION ( 'NONE',  ( 0.000000000000000000, 0.000000000000000000, -1.000000000000000000 ) ) ;
#1962 = EDGE_LOOP ( 'NONE', ( #2238, #8863, #4237, #11616, #13149 ) ) ;
#1963 = CYLINDRICAL_SURFACE ( 'NONE', #3625, 1.999999999999991340 ) ;
#1964 = DIRECTION ( 'NONE',  ( 0.000000000000000000, 0.000000000000000000, 1.000000000000000000 ) ) ;
#1965 = ADVANCED_FACE ( 'NONE', ( #10130 ), #10060, .T. ) ;
#1966 = CARTESIAN_POINT ( 'NONE',  ( 44.63563590245422574, 85.03908161011132449, 19.68933982822018081 ) ) ;
#1967 = VECTOR ( 'NONE', #10580, 1000.000000000000000 ) ;
#1968 = AXIS2_PLACEMENT_3D ( 'NONE', #4094, #12539, #7269 ) ;
#1969 = EDGE_CURVE ( 'NONE', #5251, #1420, #12949, .T. ) ;
#1970 = VERTEX_POINT ( 'NONE', #4947 ) ;
#1971 = ORIENTED_EDGE ( 'NONE', *, *, #8018, .T. ) ;
#1972 = CARTESIAN_POINT ( 'NONE',  ( -15.84264309710664165, 30.25428168447941246, 60.89715136093798975 ) ) ;
#1973 = VECTOR ( 'NONE', #3198, 1000.000000000000000 ) ;
#1974 = ORIENTED_EDGE ( 'NONE', *, *, #4373, .F. ) ;
#1975 = AXIS2_PLACEMENT_3D ( 'NONE', #5600, #11899, #2421 ) ;
#1976 = ORIENTED_EDGE ( 'NONE', *, *, #5277, .T. ) ;
#1977 = ADVANCED_FACE ( 'NONE', ( #13392 ), #4045, .T. ) ;
#1978 = FACE_OUTER_BOUND ( 'NONE', #10922, .T. ) ;
#1979 = VECTOR ( 'NONE', #86, 999.9999999999998863 ) ;
#1980 = CARTESIAN_POINT ( 'NONE',  ( -1.059188295049996231, 27.97290950744599769, 64.85000000000000853 ) ) ;
#1981 = FACE_OUTER_BOUND ( 'NONE', #13011, .T. ) ;
#1982 = ORIENTED_EDGE ( 'NONE', *, *, #9115, .T. ) ;
#1983 = DIRECTION ( 'NONE',  ( 0.000000000000000000, 0.000000000000000000, 1.000000000000000000 ) ) ;
#1984 = CARTESIAN_POINT ( 'NONE',  ( -16.40519811639460102, 9.098258476210720147, 53.85000000000000142 ) ) ;
#1985 = FACE_BOUND ( 'NONE', #12473, .T. ) ;
#1986 = DIRECTION ( 'NONE',  ( 0.000000000000000000, 0.000000000000000000, 1.000000000000000000 ) ) ;
#1987 = LINE ( 'NONE', #850, #12912 ) ;
#1988 = ADVANCED_FACE ( 'NONE', ( #8014 ), #3840, .T. ) ;
#1989 = DIRECTION ( 'NONE',  ( 0.000000000000000000, -1.000000000000000000, 0.000000000000000000 ) ) ;
#1990 = VECTOR ( 'NONE', #8575, 1000.000000000000000 ) ;
#1991 = VECTOR ( 'NONE', #12937, 1000.000000000000000 ) ;
#1992 = VECTOR ( 'NONE', #10685, 1000.000000000000000 ) ;
#1993 = VECTOR ( 'NONE', #11098, 1000.000000000000000 ) ;
#1994 = ORIENTED_EDGE ( 'NONE', *, *, #9182, .F. ) ;
#1995 = ORIENTED_EDGE ( 'NONE', *, *, #8301, .T. ) ;
#1996 = ORIENTED_EDGE ( 'NONE', *, *, #7403, .F. ) ;
#1997 = VERTEX_POINT ( 'NONE', #610 ) ;
#1998 = VERTEX_POINT ( 'NONE', #12289 ) ;
#1999 = ORIENTED_EDGE ( 'NONE', *, *, #9250, .F. ) ;
#2000 = AXIS2_PLACEMENT_3D ( 'NONE', #6057, #11507, #10460 ) ;
#2001 = TOROIDAL_SURFACE ( 'NONE', #10915, 23.29163056034262169, 0.7500000000000000000 ) ;
#2002 = VERTEX_POINT ( 'NONE', #2739 ) ;
#2003 = CIRCLE ( 'NONE', #8447, 4.750000000000000000 ) ;
#2004 = CARTESIAN_POINT ( 'NONE',  ( 68.49370948373500312, 123.0390816101113245, 19.25000000000000000 ) ) ;
#2005 = DIRECTION ( 'NONE',  ( 0.4528443260392608916, 0.8915896008669279560, 0.000000000000000000 ) ) ;
#2006 = AXIS2_PLACEMENT_3D ( 'NONE', #3693, #137, #10128 ) ;
#2007 = ORIENTED_EDGE ( 'NONE', *, *, #12117, .T. ) ;
#2008 = DIRECTION ( 'NONE',  ( 0.000000000000000000, 0.000000000000000000, 1.000000000000000000 ) ) ;
#2009 = CARTESIAN_POINT ( 'NONE',  ( -19.26123285687782172, 26.92898414971012144, 56.44653808050201604 ) ) ;
#2010 = CARTESIAN_POINT ( 'NONE',  ( -1.059188295049996231, -6.027090492554000534, 0.000000000000000000 ) ) ;
#2011 = LINE ( 'NONE', #2926, #13639 ) ;
#2012 = LINE ( 'NONE', #6454, #11612 ) ;
#2013 = DIRECTION ( 'NONE',  ( 0.000000000000000000, 0.000000000000000000, 1.000000000000000000 ) ) ;
#2014 = VERTEX_POINT ( 'NONE', #1453 ) ;
#2015 = ORIENTED_EDGE ( 'NONE', *, *, #4918, .T. ) ;
#2016 = EDGE_CURVE ( 'NONE', #6494, #5283, #8089, .T. ) ;
#2017 = AXIS2_PLACEMENT_3D ( 'NONE', #1910, #5941, #784 ) ;
#2018 = AXIS2_PLACEMENT_3D ( 'NONE', #10654, #10728, #1016 ) ;
#2019 = ORIENTED_EDGE ( 'NONE', *, *, #5327, .T. ) ;
#2020 = DIRECTION ( 'NONE',  ( 1.000000000000000000, 0.000000000000000000, 0.000000000000000000 ) ) ;
#2021 = LINE ( 'NONE', #12407, #2187 ) ;
#2022 = ORIENTED_EDGE ( 'NONE', *, *, #5657, .T. ) ;
#2023 = DIRECTION ( 'NONE',  ( 0.000000000000000000, 0.000000000000000000, -1.000000000000000000 ) ) ;
#2024 = LINE ( 'NONE', #4038, #1266 ) ;
#2025 = CARTESIAN_POINT ( 'NONE',  ( -35.05918829505000645, 27.97290950744599769, 17.25000000000000000 ) ) ;
#2026 = DIRECTION ( 'NONE',  ( 1.000000000000000000, 0.000000000000000000, 0.000000000000000000 ) ) ;
#2027 = FACE_OUTER_BOUND ( 'NONE', #12665, .T. ) ;
#2028 = DIRECTION ( 'NONE',  ( 0.000000000000000000, 0.000000000000000000, 1.000000000000000000 ) ) ;
#2029 = CARTESIAN_POINT ( 'NONE',  ( 16.04064420431708982, 0.000000000000000000, 11.30758658292212893 ) ) ;
#2030 = DIRECTION ( 'NONE',  ( -1.000000000000000000, 0.000000000000000000, 0.000000000000000000 ) ) ;
#2031 = AXIS2_PLACEMENT_3D ( 'NONE', #5718, #1330, #13065 ) ;
#2032 = CARTESIAN_POINT ( 'NONE',  ( -1.059188295049996231, 27.97290950744599769, 0.000000000000000000 ) ) ;
#2033 = AXIS2_PLACEMENT_3D ( 'NONE', #8135, #12344, #5129 ) ;
#2034 = EDGE_CURVE ( 'NONE', #13684, #9242, #6963, .T. ) ;
#2035 = ORIENTED_EDGE ( 'NONE', *, *, #11360, .T. ) ;
#2036 = VERTEX_POINT ( 'NONE', #12359 ) ;
#2037 = LINE ( 'NONE', #6122, #4591 ) ;
#2038 = VECTOR ( 'NONE', #10861, 1000.000000000000000 ) ;
#2039 = AXIS2_PLACEMENT_3D ( 'NONE', #6487, #8723, #8393 ) ;
#2040 = ORIENTED_EDGE ( 'NONE', *, *, #12628, .F. ) ;
#2041 = ORIENTED_EDGE ( 'NONE', *, *, #8256, .F. ) ;
#2042 = DIRECTION ( 'NONE',  ( 0.000000000000000000, 0.000000000000000000, -1.000000000000000000 ) ) ;
#2043 = DIRECTION ( 'NONE',  ( 0.000000000000000000, -0.000000000000000000, -1.000000000000000000 ) ) ;
#2044 = FACE_OUTER_BOUND ( 'NONE', #10676, .T. ) ;
#2045 = DIRECTION ( 'NONE',  ( 0.000000000000000000, 0.000000000000000000, -1.000000000000000000 ) ) ;
#2046 = CARTESIAN_POINT ( 'NONE',  ( -18.05918829504999934, 14.81548537210212046, 5.250000000000000000 ) ) ;
#2047 = AXIS2_PLACEMENT_3D ( 'NONE', #10452, #880, #5138 ) ;
#2048 = VECTOR ( 'NONE', #8009, 1000.000000000000000 ) ;
#2049 = AXIS2_PLACEMENT_3D ( 'NONE', #4747, #1518, #5774 ) ;
#2050 = ADVANCED_FACE ( 'NONE', ( #11238 ), #4679, .F. ) ;
#2051 = CARTESIAN_POINT ( 'NONE',  ( -14.69313762561336212, 30.11514052169665590, 55.27969735402319884 ) ) ;
#2052 = ORIENTED_EDGE ( 'NONE', *, *, #10164, .F. ) ;
#2053 = ORIENTED_EDGE ( 'NONE', *, *, #4933, .F. ) ;
#2054 = DIRECTION ( 'NONE',  ( 0.4678190685372707325, -0.5302313826179287926, 0.7071067811865475727 ) ) ;
#2055 = ADVANCED_FACE ( 'NONE', ( #2806 ), #5586, .F. ) ;
#2056 = AXIS2_PLACEMENT_3D ( 'NONE', #8028, #13265, #8803 ) ;
#2057 = AXIS2_PLACEMENT_3D ( 'NONE', #13251, #3691, #7934 ) ;
#2058 = CARTESIAN_POINT ( 'NONE',  ( -25.86749127492460332, 30.80589556422609476, 83.57661607529820458 ) ) ;
#2059 = ORIENTED_EDGE ( 'NONE', *, *, #3701, .T. ) ;
#2060 = DIRECTION ( 'NONE',  ( -0.000000000000000000, -0.000000000000000000, 1.000000000000000000 ) ) ;
#2061 = DIRECTION ( 'NONE',  ( 0.000000000000000000, 0.000000000000000000, -1.000000000000000000 ) ) ;
#2062 = DIRECTION ( 'NONE',  ( 0.000000000000000000, -1.000000000000000000, 0.000000000000000000 ) ) ;
#2063 = DIRECTION ( 'NONE',  ( 0.000000000000000000, 0.000000000000000000, -1.000000000000000000 ) ) ;
#2064 = EDGE_CURVE ( 'NONE', #10722, #5219, #5804, .T. ) ;
#2065 = VECTOR ( 'NONE', #4779, 1000.000000000000000 ) ;
#2066 = CIRCLE ( 'NONE', #9871, 34.69999999999999574 ) ;
#2067 = ORIENTED_EDGE ( 'NONE', *, *, #13210, .F. ) ;
#2068 = ORIENTED_EDGE ( 'NONE', *, *, #1780, .F. ) ;
#2069 = ORIENTED_EDGE ( 'NONE', *, *, #6084, .F. ) ;
#2070 = ORIENTED_EDGE ( 'NONE', *, *, #9844, .F. ) ;
#2071 = EDGE_CURVE ( 'NONE', #4627, #533, #8283, .T. ) ;
#2072 = EDGE_CURVE ( 'NONE', #12394, #2952, #10265, .T. ) ;
#2073 = DIRECTION ( 'NONE',  ( -0.6615960714621564875, 0.7498604124941129490, 0.000000000000000000 ) ) ;
#2074 = DIRECTION ( 'NONE',  ( 1.049727191138617833E-16, 0.5150380749100549327, -0.8571673007021118895 ) ) ;
#2075 = VERTEX_POINT ( 'NONE', #2597 ) ;
#2076 = CARTESIAN_POINT ( 'NONE',  ( 44.73918929304747394, 94.80194462843097369, 23.00000000000000000 ) ) ;
#2077 = AXIS2_PLACEMENT_3D ( 'NONE', #6263, #10806, #4378 ) ;
#2078 = DIRECTION ( 'NONE',  ( 0.000000000000000000, 1.000000000000000000, -0.000000000000000000 ) ) ;
#2079 = CYLINDRICAL_SURFACE ( 'NONE', #11541, 0.2500000000000002220 ) ;
#2080 = CARTESIAN_POINT ( 'NONE',  ( -10.44110272205000101, 10.97290950744599947, 61.65955166399999854 ) ) ;
#2081 = DIRECTION ( 'NONE',  ( 0.000000000000000000, 0.000000000000000000, 1.000000000000000000 ) ) ;
#2082 = VERTEX_POINT ( 'NONE', #1595 ) ;
#2083 = CIRCLE ( 'NONE', #10773, 1.999999999999994893 ) ;
#2084 = VERTEX_POINT ( 'NONE', #3906 ) ;
#2085 = LINE ( 'NONE', #11706, #7244 ) ;
#2086 = CARTESIAN_POINT ( 'NONE',  ( 92.63563590245421153, 112.2890816101113387, 0.000000000000000000 ) ) ;
#2087 = ORIENTED_EDGE ( 'NONE', *, *, #8859, .T. ) ;
#2088 = CARTESIAN_POINT ( 'NONE',  ( -36.05918829505000645, 10.97290950744599947, 63.45000000000000284 ) ) ;
#2089 = CARTESIAN_POINT ( 'NONE',  ( 62.16596598834446752, 129.5087515242215090, 0.7500000000000000000 ) ) ;
#2090 = CARTESIAN_POINT ( 'NONE',  ( -0.3963656581980404825, 10.97290950744599947, 6.250000000000000000 ) ) ;
#2091 = FILL_AREA_STYLE_COLOUR ( '', #10994 ) ;
#2092 = CARTESIAN_POINT ( 'NONE',  ( -5.173045190668890569, -15.68519459986890041, 5.250000000000000000 ) ) ;
#2093 = FACE_OUTER_BOUND ( 'NONE', #10375, .T. ) ;
#2094 = ADVANCED_FACE ( 'NONE', ( #12416 ), #6766, .F. ) ;
#2095 = CARTESIAN_POINT ( 'NONE',  ( -25.05563313235659706, -2.802149825948039741, 57.35000000000000142 ) ) ;
#2096 = CIRCLE ( 'NONE', #13448, 0.9499999999999995115 ) ;
#2097 = CYLINDRICAL_SURFACE ( 'NONE', #13596, 4.750000000000000888 ) ;
#2098 =( LENGTH_UNIT ( ) NAMED_UNIT ( * ) SI_UNIT ( .MILLI., .METRE. ) );
#2099 = ORIENTED_EDGE ( 'NONE', *, *, #8375, .F. ) ;
#2100 = EDGE_LOOP ( 'NONE', ( #1916, #2103, #11395, #3232 ) ) ;
#2101 = TOROIDAL_SURFACE ( 'NONE', #4765, 10.75000000000000000, 0.7500000000000000000 ) ;
#2102 = FACE_OUTER_BOUND ( 'NONE', #11298, .T. ) ;
#2103 = ORIENTED_EDGE ( 'NONE', *, *, #7329, .F. ) ;
#2104 = ORIENTED_EDGE ( 'NONE', *, *, #2194, .F. ) ;
#2105 = VERTEX_POINT ( 'NONE', #11100 ) ;
#2106 = DIRECTION ( 'NONE',  ( -1.000000000000000000, 0.000000000000000000, 0.000000000000000000 ) ) ;
#2107 = CARTESIAN_POINT ( 'NONE',  ( 116.7775623211734342, 113.0390816101113387, 20.00000000000000000 ) ) ;
#2108 = DIRECTION ( 'NONE',  ( 1.000000000000000000, 0.000000000000000000, 0.000000000000000000 ) ) ;
#2110 = ORIENTED_EDGE ( 'NONE', *, *, #9459, .T. ) ;
#2109 = EDGE_CURVE ( 'NONE', #10331, #1179, #3825, .T. ) ;
#2111 = CARTESIAN_POINT ( 'NONE',  ( -16.03669512066808878, 6.089431995824910793, 68.56428208524678780 ) ) ;
#2112 = ADVANCED_FACE ( 'NONE', ( #9004 ), #12213, .T. ) ;
#2113 = DIRECTION ( 'NONE',  ( 0.000000000000000000, 0.000000000000000000, -1.000000000000000000 ) ) ;
#2114 = ADVANCED_FACE ( 'NONE', ( #886 ), #7167, .T. ) ;
#2115 = CARTESIAN_POINT ( 'NONE',  ( -18.05918829504999934, 10.97290950744599947, 62.14999999999999858 ) ) ;
#2116 = EDGE_LOOP ( 'NONE', ( #911, #6984, #11746, #6787 ) ) ;
#2117 = EDGE_LOOP ( 'NONE', ( #1870, #3117, #10090, #5500, #145, #13107 ) ) ;
#2118 = ORIENTED_EDGE ( 'NONE', *, *, #10161, .F. ) ;
#2119 = DIRECTION ( 'NONE',  ( -0.000000000000000000, -1.000000000000000000, 0.000000000000000000 ) ) ;
#2120 =( NAMED_UNIT ( * ) SI_UNIT ( $, .STERADIAN. ) SOLID_ANGLE_UNIT ( ) );
#2121 = DIRECTION ( 'NONE',  ( 0.000000000000000000, 0.000000000000000000, -1.000000000000000000 ) ) ;
#2122 = DIRECTION ( 'NONE',  ( 1.000000000000000000, 0.000000000000000000, 0.000000000000000000 ) ) ;
#2123 = FACE_BOUND ( 'NONE', #3187, .T. ) ;
#2124 = EDGE_CURVE ( 'NONE', #4612, #4329, #10080, .T. ) ;
#2125 = EDGE_CURVE ( 'NONE', #7771, #13568, #7363, .T. ) ;
#2126 = DIRECTION ( 'NONE',  ( -0.4528443260392610026, -0.8915896008669278450, 0.000000000000000000 ) ) ;
#2127 = EDGE_CURVE ( 'NONE', #9316, #10025, #6114, .T. ) ;
#2128 = DIRECTION ( 'NONE',  ( 0.000000000000000000, 0.000000000000000000, -1.000000000000000000 ) ) ;
#2129 = ADVANCED_FACE ( 'NONE', ( #13670, #811 ), #1809, .F. ) ;
#2130 = ORIENTED_EDGE ( 'NONE', *, *, #5610, .T. ) ;
#2131 = ORIENTED_EDGE ( 'NONE', *, *, #12002, .T. ) ;
#2132 = ORIENTED_EDGE ( 'NONE', *, *, #5350, .T. ) ;
#2133 = ORIENTED_EDGE ( 'NONE', *, *, #6193, .T. ) ;
#2134 = EDGE_LOOP ( 'NONE', ( #8813, #10347 ) ) ;
#2135 = CLOSED_SHELL ( 'NONE', ( #10986, #4360, #4734, #1977, #11427, #9285, #12252, #2793, #13511, #4146, #8949, #2966, #4475, #282, #1182, #2890, #9514, #7397, #9351, #9390, #1023, #7312, #701, #1959, #11279, #11167, #4130 ) ) ;
#2136 = CARTESIAN_POINT ( 'NONE',  ( -0.05918829504999999908, 10.97290950744599947, 62.14999999999999858 ) ) ;
#2137 = LINE ( 'NONE', #9464, #13121 ) ;
#2138 = EDGE_CURVE ( 'NONE', #12260, #2002, #4117, .T. ) ;
#2139 = ORIENTED_EDGE ( 'NONE', *, *, #3841, .F. ) ;
#2140 = CARTESIAN_POINT ( 'NONE',  ( -18.05918829504999934, 10.97290950744599947, 63.54999999999999716 ) ) ;
#2141 = DIRECTION ( 'NONE',  ( -0.4528443260392611136, -0.8915896008669277339, 0.000000000000000000 ) ) ;
#2142 = CYLINDRICAL_SURFACE ( 'NONE', #11765, 3.000000000000002665 ) ;
#2143 = CYLINDRICAL_SURFACE ( 'NONE', #5999, 6.000000000000002665 ) ;
#2144 = CIRCLE ( 'NONE', #1676, 16.75000000000000355 ) ;
#2145 = CYLINDRICAL_SURFACE ( 'NONE', #3565, 6.000000000000000888 ) ;
#2146 = CONTEXT_DEPENDENT_SHAPE_REPRESENTATION ( #2902, #12172 ) ;
#2147 = ORIENTED_EDGE ( 'NONE', *, *, #2760, .F. ) ;
#2148 = ADVANCED_FACE ( 'NONE', ( #11652 ), #749, .F. ) ;
#2149 = VERTEX_POINT ( 'NONE', #2029 ) ;
#2150 = VECTOR ( 'NONE', #11865, 1000.000000000000227 ) ;
#2151 = CARTESIAN_POINT ( 'NONE',  ( 4.500000000000002665, -0.5000000000000005551, -65.00000000000000000 ) ) ;
#2152 = LINE ( 'NONE', #12953, #13752 ) ;
#2153 = LINE ( 'NONE', #4239, #9391 ) ;
#2154 = DIRECTION ( 'NONE',  ( 1.000000000000000000, 0.000000000000000000, 0.000000000000000000 ) ) ;
#2155 = CARTESIAN_POINT ( 'NONE',  ( -19.45034526138887188, 30.31858837287976272, 53.29192511634208529 ) ) ;
#2156 = CARTESIAN_POINT ( 'NONE',  ( -11.74835982676941981, -4.028726038184999858, 62.14999999999999858 ) ) ;
#2157 = ORIENTED_EDGE ( 'NONE', *, *, #3698, .T. ) ;
#2158 = CARTESIAN_POINT ( 'NONE',  ( -21.16117192841894834, 4.865520741507539881, 61.25000000000000000 ) ) ;
#2159 = CARTESIAN_POINT ( 'NONE',  ( -39.30918829504999934, 27.97290950744599769, 58.85000000000000142 ) ) ;
#2160 = DIRECTION ( 'NONE',  ( 0.000000000000000000, 1.000000000000000000, 0.000000000000000000 ) ) ;
#2161 = FACE_BOUND ( 'NONE', #12086, .T. ) ;
#2162 =( NAMED_UNIT ( * ) SI_UNIT ( $, .STERADIAN. ) SOLID_ANGLE_UNIT ( ) );
#2163 = CIRCLE ( 'NONE', #11729, 6.000000000000005329 ) ;
#2164 = EDGE_CURVE ( 'NONE', #2876, #11929, #5009, .T. ) ;
#2165 = EDGE_CURVE ( 'NONE', #1164, #11479, #13593, .T. ) ;
#2166 = EDGE_LOOP ( 'NONE', ( #3453, #7119, #2202, #7275 ) ) ;
#2167 = DIRECTION ( 'NONE',  ( 0.4528443260392608360, 0.8915896008669278450, 0.000000000000000000 ) ) ;
#2168 = ORIENTED_EDGE ( 'NONE', *, *, #126, .T. ) ;
#2169 = ORIENTED_EDGE ( 'NONE', *, *, #8109, .T. ) ;
#2170 = DIRECTION ( 'NONE',  ( 0.000000000000000000, 0.000000000000000000, 1.000000000000000000 ) ) ;
#2171 = VECTOR ( 'NONE', #1183, 1000.000000000000000 ) ;
#2172 = DIRECTION ( 'NONE',  ( 1.000000000000000000, 0.000000000000000000, 0.000000000000000000 ) ) ;
#2173 = DIRECTION ( 'NONE',  ( 0.000000000000000000, 0.000000000000000000, -1.000000000000000000 ) ) ;
#2174 = CYLINDRICAL_SURFACE ( 'NONE', #11564, 1.999999999999991340 ) ;
#2175 = DIRECTION ( 'NONE',  ( 1.000000000000000000, 0.000000000000000000, 0.000000000000000000 ) ) ;
#2176 =( REPRESENTATION_RELATIONSHIP ('NONE','NONE', #11848, #5502 ) REPRESENTATION_RELATIONSHIP_WITH_TRANSFORMATION ( #10520 )SHAPE_REPRESENTATION_RELATIONSHIP( ) );
#2177 = CIRCLE ( 'NONE', #11750, 33.00000000000000000 ) ;
#2178 = EDGE_CURVE ( 'NONE', #7807, #7753, #19, .T. ) ;
#2179 = ORIENTED_EDGE ( 'NONE', *, *, #3469, .T. ) ;
#2180 = EDGE_CURVE ( 'NONE', #10750, #586, #4056, .T. ) ;
#2181 = CARTESIAN_POINT ( 'NONE',  ( -15.53293347889121989, 30.22252884722569988, 54.08287280684341880 ) ) ;
#2182 = ORIENTED_EDGE ( 'NONE', *, *, #2264, .T. ) ;
#2183 = VERTEX_POINT ( 'NONE', #10595 ) ;
#2184 = ORIENTED_EDGE ( 'NONE', *, *, #13109, .F. ) ;
#2185 = DIRECTION ( 'NONE',  ( 0.000000000000000000, 0.000000000000000000, -1.000000000000000000 ) ) ;
#2186 = DIRECTION ( 'NONE',  ( 1.000000000000000000, 0.000000000000000000, 0.000000000000000000 ) ) ;
#2187 = VECTOR ( 'NONE', #955, 1000.000000000000000 ) ;
#2188 = DIRECTION ( 'NONE',  ( -0.7071067811865451302, 0.7071067811865500152, 0.000000000000000000 ) ) ;
#2189 = VERTEX_POINT ( 'NONE', #1022 ) ;
#2190 = DIRECTION ( 'NONE',  ( 0.000000000000000000, 0.000000000000000000, 1.000000000000000000 ) ) ;
#2191 = FACE_OUTER_BOUND ( 'NONE', #2483, .T. ) ;
#2192 = CYLINDRICAL_SURFACE ( 'NONE', #12922, 0.2500000000000002220 ) ;
#2193 = DIRECTION ( 'NONE',  ( 0.000000000000000000, 0.000000000000000000, -1.000000000000000000 ) ) ;
#2194 = EDGE_CURVE ( 'NONE', #2935, #703, #11852, .T. ) ;
#2195 = CIRCLE ( 'NONE', #1731, 16.99999999999999645 ) ;
#2196 = CIRCLE ( 'NONE', #9998, 2.500000000000000000 ) ;
#2197 = ORIENTED_EDGE ( 'NONE', *, *, #12092, .F. ) ;
#2198 = EDGE_CURVE ( 'NONE', #2014, #4562, #3383, .T. ) ;
#2199 = AXIS2_PLACEMENT_3D ( 'NONE', #6743, #7914, #12263 ) ;
#2200 = ORIENTED_EDGE ( 'NONE', *, *, #3509, .F. ) ;
#2201 = FACE_OUTER_BOUND ( 'NONE', #12238, .T. ) ;
#2202 = ORIENTED_EDGE ( 'NONE', *, *, #718, .T. ) ;
#2203 = ORIENTED_EDGE ( 'NONE', *, *, #9709, .F. ) ;
#2204 = ORIENTED_EDGE ( 'NONE', *, *, #6665, .F. ) ;
#2205 = CARTESIAN_POINT ( 'NONE',  ( 8.500000000000003553, 2.500000000000000000, 0.000000000000000000 ) ) ;
#2206 = LINE ( 'NONE', #9670, #6872 ) ;
#2207 = PRODUCT_DEFINITION ( 'UNKNOWN', '', #12909, #7100 ) ;
#2208 = EDGE_LOOP ( 'NONE', ( #3202, #4187, #8745, #10570 ) ) ;
#2209 = DIRECTION ( 'NONE',  ( 0.000000000000000000, 0.000000000000000000, -1.000000000000000000 ) ) ;
#2210 = FACE_OUTER_BOUND ( 'NONE', #2874, .T. ) ;
#2211 = CIRCLE ( 'NONE', #10005, 4.750000000000000888 ) ;
#2212 = DIRECTION ( 'NONE',  ( 0.000000000000000000, 0.000000000000000000, 1.000000000000000000 ) ) ;
#2213 = DIRECTION ( 'NONE',  ( 0.000000000000000000, 0.000000000000000000, 1.000000000000000000 ) ) ;
#2214 = CIRCLE ( 'NONE', #11556, 24.92993838181874722 ) ;
#2215 = CARTESIAN_POINT ( 'NONE',  ( 140.6356359024541973, 94.90549801902425031, 22.75000000000000000 ) ) ;
#2216 = CONTEXT_DEPENDENT_SHAPE_REPRESENTATION ( #5014, #7922 ) ;
#2217 = ADVANCED_FACE ( 'NONE', ( #7093 ), #4247, .T. ) ;
#2218 = AXIS2_PLACEMENT_3D ( 'NONE', #2537, #2600, #11166 ) ;
#2219 = VECTOR ( 'NONE', #9243, 1000.000000000000000 ) ;
#2220 = VECTOR ( 'NONE', #4246, 1000.000000000000000 ) ;
#2221 = VERTEX_POINT ( 'NONE', #9424 ) ;
#2222 = DIRECTION ( 'NONE',  ( 0.000000000000000000, 0.000000000000000000, 1.000000000000000000 ) ) ;
#2223 = CARTESIAN_POINT ( 'NONE',  ( -35.05918829505000645, 27.97290950744599769, 58.85000000000000142 ) ) ;
#2224 = FACE_OUTER_BOUND ( 'NONE', #6481, .T. ) ;
#2225 = CARTESIAN_POINT ( 'NONE',  ( 0.000000000000000000, 94.65549801902425031, 22.75000000000000000 ) ) ;
#2226 = EDGE_CURVE ( 'NONE', #6329, #9971, #2870, .T. ) ;
#2227 = CARTESIAN_POINT ( 'NONE',  ( 109.6856792294029219, 82.08927268643400055, 19.25000000000000000 ) ) ;
#2228 = DIRECTION ( 'NONE',  ( 0.000000000000000000, 0.000000000000000000, 1.000000000000000000 ) ) ;
#2229 = EDGE_LOOP ( 'NONE', ( #12559, #13234, #6292, #1717 ) ) ;
#2230 = CARTESIAN_POINT ( 'NONE',  ( -26.45502162804999813, 10.97290950744599947, 60.04999999999999716 ) ) ;
#2231 = DIRECTION ( 'NONE',  ( 0.000000000000000000, 0.000000000000000000, -1.000000000000000000 ) ) ;
#2232 = DIRECTION ( 'NONE',  ( 0.000000000000000000, 0.000000000000000000, 1.000000000000000000 ) ) ;
#2233 = CARTESIAN_POINT ( 'NONE',  ( -1.059188295049996231, 27.97290950744599769, 68.85549045786049760 ) ) ;
#2234 = AXIS2_PLACEMENT_3D ( 'NONE', #13029, #3474, #9620 ) ;
#2235 = EDGE_CURVE ( 'NONE', #10451, #8158, #11439, .T. ) ;
#2236 = SHAPE_REPRESENTATION ( 'Rotary Faceplate', ( #6434 ), #2686 ) ;
#2237 = LINE ( 'NONE', #8567, #1014 ) ;
#2238 = ORIENTED_EDGE ( 'NONE', *, *, #8018, .F. ) ;
#2239 = ORIENTED_EDGE ( 'NONE', *, *, #7229, .F. ) ;
#2240 = EDGE_LOOP ( 'NONE', ( #8583, #3718, #310, #1759 ) ) ;
#2241 = EDGE_LOOP ( 'NONE', ( #12437, #1063, #6773, #2916 ) ) ;
#2242 = ORIENTED_EDGE ( 'NONE', *, *, #11842, .T. ) ;
#2243 = CARTESIAN_POINT ( 'NONE',  ( -39.30918829504999934, 27.97290950744599769, 64.85000000000000853 ) ) ;
#2244 = EDGE_CURVE ( 'NONE', #912, #8943, #10521, .T. ) ;
#2245 = CARTESIAN_POINT ( 'NONE',  ( 8.500000000000001776, 2.000000000000000000, -65.00000000000000000 ) ) ;
#2246 = AXIS2_PLACEMENT_3D ( 'NONE', #77, #11683, #994 ) ;
#2247 = VECTOR ( 'NONE', #1159, 1000.000000000000000 ) ;
#2248 = PLANE ( 'NONE',  #2969 ) ;
#2249 = CARTESIAN_POINT ( 'NONE',  ( 1.940811704950003991, 27.97290950744599769, 0.000000000000000000 ) ) ;
#2250 = CARTESIAN_POINT ( 'NONE',  ( -18.05918829504999934, 10.97290950744599947, 60.60999999999999943 ) ) ;
#2251 = CARTESIAN_POINT ( 'NONE',  ( -10.78334210919089919, 29.19143287883919768, 7.250000000000000000 ) ) ;
#2252 = CARTESIAN_POINT ( 'NONE',  ( 27.50000000000001066, 0.000000000000000000, 29.99999999999999645 ) ) ;
#2253 = UNCERTAINTY_MEASURE_WITH_UNIT (LENGTH_MEASURE( 1.000000000000000082E-05 ), #2308, 'distance_accuracy_value', 'NONE');
#2254 = CIRCLE ( 'NONE', #7334, 2.500000000000000000 ) ;
#2255 = PRODUCT ( 'Central Rotary Housing', 'Central Rotary Housing', '', ( #4306 ) ) ;
#2256 = CIRCLE ( 'NONE', #5566, 1.725000000000000755 ) ;
#2257 = VERTEX_POINT ( 'NONE', #10663 ) ;
#2258 = CARTESIAN_POINT ( 'NONE',  ( -15.80213232358579667, 30.25036691325134797, 53.83618312000469786 ) ) ;
#2259 = ORIENTED_EDGE ( 'NONE', *, *, #544, .F. ) ;
#2260 = ORIENTED_EDGE ( 'NONE', *, *, #11265, .F. ) ;
#2261 = ORIENTED_EDGE ( 'NONE', *, *, #12459, .T. ) ;
#2262 = DIRECTION ( 'NONE',  ( 0.000000000000000000, 0.000000000000000000, 1.000000000000000000 ) ) ;
#2263 = DIRECTION ( 'NONE',  ( -1.000000000000000000, -0.000000000000000000, -0.000000000000000000 ) ) ;
#2264 = EDGE_CURVE ( 'NONE', #12897, #9534, #6600, .T. ) ;
#2265 =( LENGTH_UNIT ( ) NAMED_UNIT ( * ) SI_UNIT ( .MILLI., .METRE. ) );
#2266 = VERTEX_POINT ( 'NONE', #6674 ) ;
#2267 = CARTESIAN_POINT ( 'NONE',  ( 140.6356359024541973, 113.0390816101113387, 0.7500000000000006661 ) ) ;
#2268 = CARTESIAN_POINT ( 'NONE',  ( -18.05918829504999934, 10.97290950744599947, 62.14999999999999858 ) ) ;
#2269 = CIRCLE ( 'NONE', #12058, 3.000000000000000000 ) ;
#2270 = VECTOR ( 'NONE', #2974, 1000.000000000000000 ) ;
#2271 = AXIS2_PLACEMENT_3D ( 'NONE', #2778, #4843, #1845 ) ;
#2272 = AXIS2_PLACEMENT_3D ( 'NONE', #7060, #12387, #782 ) ;
#2273 = DIRECTION ( 'NONE',  ( 0.000000000000000000, 0.000000000000000000, -1.000000000000000000 ) ) ;
#2274 = EDGE_CURVE ( 'NONE', #4079, #1491, #4720, .T. ) ;
#2275 = FACE_OUTER_BOUND ( 'NONE', #13006, .T. ) ;
#2276 = EDGE_LOOP ( 'NONE', ( #634, #6515 ) ) ;
#2277 = CIRCLE ( 'NONE', #7357, 0.9499999999999995115 ) ;
#2278 = VECTOR ( 'NONE', #6055, 1000.000000000000000 ) ;
#2279 = VERTEX_POINT ( 'NONE', #3476 ) ;
#2280 = ORIENTED_EDGE ( 'NONE', *, *, #3168, .T. ) ;
#2281 = DIRECTION ( 'NONE',  ( -0.000000000000000000, -0.000000000000000000, 1.000000000000000000 ) ) ;
#2282 = DIRECTION ( 'NONE',  ( 0.000000000000000000, 0.000000000000000000, -1.000000000000000000 ) ) ;
#2283 = ORIENTED_EDGE ( 'NONE', *, *, #8978, .F. ) ;
#2284 = CARTESIAN_POINT ( 'NONE',  ( 44.63563590245420443, 94.90549801902425031, 22.75000000000000000 ) ) ;
#2285 = DIRECTION ( 'NONE',  ( -0.000000000000000000, -0.000000000000000000, -1.000000000000000000 ) ) ;
#2286 = LINE ( 'NONE', #7466, #1973 ) ;
#2287 = FACE_OUTER_BOUND ( 'NONE', #4614, .T. ) ;
#2288 = EDGE_CURVE ( 'NONE', #10798, #2353, #1355, .T. ) ;
#2289 = DIRECTION ( 'NONE',  ( -0.000000000000000000, -0.000000000000000000, -1.000000000000000000 ) ) ;
#2290 = COLOUR_RGB ( '', 0.31764706, 0.68627451, 0.89019608) ;
#2291 = APPLICATION_PROTOCOL_DEFINITION ( 'draft international standard', 'automotive_design', 1998, #8055 ) ;
#2292 = EDGE_LOOP ( 'NONE', ( #580, #3180, #12636, #7033 ) ) ;
#2293 = CIRCLE ( 'NONE', #1600, 4.750000000000000888 ) ;
#2294 = ORIENTED_EDGE ( 'NONE', *, *, #6998, .F. ) ;
#2295 = ORIENTED_EDGE ( 'NONE', *, *, #6049, .T. ) ;
#2296 = VERTEX_POINT ( 'NONE', #10876 ) ;
#2297 = CIRCLE ( 'NONE', #698, 4.250000000000000000 ) ;
#2298 = CARTESIAN_POINT ( 'NONE',  ( -38.05918829505000645, -6.027090492554000534, 0.000000000000000000 ) ) ;
#2299 = EDGE_LOOP ( 'NONE', ( #666, #3811 ) ) ;
#2300 = LINE ( 'NONE', #6535, #12959 ) ;
#2301 = CARTESIAN_POINT ( 'NONE',  ( -20.84461927375554779, 30.19267137841694293, 54.36848034354279946 ) ) ;
#2302 = LINE ( 'NONE', #11772, #1160 ) ;
#2303 = LINE ( 'NONE', #11921, #9799 ) ;
#2304 = CYLINDRICAL_SURFACE ( 'NONE', #8227, 0.2500000000000002220 ) ;
#2305 = CYLINDRICAL_SURFACE ( 'NONE', #5365, 8.299999999999998934 ) ;
#2306 = EDGE_CURVE ( 'NONE', #4291, #159, #7705, .T. ) ;
#2307 = CARTESIAN_POINT ( 'NONE',  ( -40.05918829504999934, -14.02709049255400053, 0.000000000000000000 ) ) ;
#2308 =( LENGTH_UNIT ( ) NAMED_UNIT ( * ) SI_UNIT ( .MILLI., .METRE. ) );
#2309 = EDGE_CURVE ( 'NONE', #4982, #11879, #8778, .T. ) ;
#2310 = VECTOR ( 'NONE', #10660, 1000.000000000000000 ) ;
#2311 = EDGE_CURVE ( 'NONE', #189, #8669, #6714, .T. ) ;
#2312 = EDGE_LOOP ( 'NONE', ( #12395, #12524, #11737, #10650 ) ) ;
#2313 = ORIENTED_EDGE ( 'NONE', *, *, #9180, .F. ) ;
#2314 = DIRECTION ( 'NONE',  ( 0.000000000000000000, 0.000000000000000000, 1.000000000000000000 ) ) ;
#2315 = ORIENTED_EDGE ( 'NONE', *, *, #7940, .T. ) ;
#2316 = ORIENTED_EDGE ( 'NONE', *, *, #1679, .F. ) ;
#2317 = ORIENTED_EDGE ( 'NONE', *, *, #8020, .T. ) ;
#2318 = ORIENTED_EDGE ( 'NONE', *, *, #13401, .T. ) ;
#2319 = DIRECTION ( 'NONE',  ( 0.000000000000000000, 0.000000000000000000, 1.000000000000000000 ) ) ;
#2320 = AXIS2_PLACEMENT_3D ( 'NONE', #8544, #9673, #7465 ) ;
#2321 = PRODUCT_DEFINITION_SHAPE ( 'NONE', 'NONE',  #9627 ) ;
#2322 = LINE ( 'NONE', #480, #13616 ) ;
#2323 = SURFACE_STYLE_FILL_AREA ( #6349 ) ;
#2324 = CARTESIAN_POINT ( 'NONE',  ( 0.000000000000000000, 0.000000000000000000, 17.25000000000000000 ) ) ;
#2325 = CARTESIAN_POINT ( 'NONE',  ( 116.7775623211734342, 85.03908161011133870, 0.000000000000000000 ) ) ;
#2326 = EDGE_CURVE ( 'NONE', #1970, #9632, #4494, .T. ) ;
#2327 = DIRECTION ( 'NONE',  ( 0.9496839325805418452, -0.3132098788326394545, 0.000000000000000000 ) ) ;
#2328 = DIRECTION ( 'NONE',  ( 0.000000000000000000, 0.000000000000000000, -1.000000000000000000 ) ) ;
#2329 =( BOUNDED_CURVE ( )  B_SPLINE_CURVE ( 3, ( #11502, #3964, #13460, #11369 ),
 .UNSPECIFIED., .F., .F. ) 
 B_SPLINE_CURVE_WITH_KNOTS ( ( 4, 4 ),
 ( 3.141592653589793116, 4.712388980384689674 ),
 .UNSPECIFIED. ) 
 CURVE ( )  GEOMETRIC_REPRESENTATION_ITEM ( )  RATIONAL_B_SPLINE_CURVE ( ( 1.000000000000000000, 0.8047378541243649375, 0.8047378541243649375, 1.000000000000000000 ) ) 
 REPRESENTATION_ITEM ( '' )  );
#2330 = EDGE_CURVE ( 'NONE', #3796, #4496, #9836, .T. ) ;
#2331 = CIRCLE ( 'NONE', #12781, 16.50000000000000000 ) ;
#2332 = ORIENTED_EDGE ( 'NONE', *, *, #9772, .F. ) ;
#2333 = ORIENTED_EDGE ( 'NONE', *, *, #1546, .T. ) ;
#2334 = CARTESIAN_POINT ( 'NONE',  ( -16.46704392475020384, 30.30564942409548834, 53.38979243784910267 ) ) ;
#2335 = ORIENTED_EDGE ( 'NONE', *, *, #6802, .T. ) ;
#2336 = LINE ( 'NONE', #3365, #10855 ) ;
#2337 = LINE ( 'NONE', #12992, #7804 ) ;
#2338 = DIRECTION ( 'NONE',  ( 0.000000000000000000, 0.000000000000000000, 1.000000000000000000 ) ) ;
#2339 = VECTOR ( 'NONE', #5975, 1000.000000000000000 ) ;
#2340 = CARTESIAN_POINT ( 'NONE',  ( -18.05918829504999934, 19.05294282444599929, 63.34900083300000517 ) ) ;
#2341 = DIRECTION ( 'NONE',  ( 0.000000000000000000, -0.000000000000000000, 1.000000000000000000 ) ) ;
#2342 = EDGE_CURVE ( 'NONE', #172, #6605, #2501, .T. ) ;
#2343 = EDGE_CURVE ( 'NONE', #8943, #1848, #244, .T. ) ;
#2344 = EDGE_CURVE ( 'NONE', #5817, #3979, #7816, .T. ) ;
#2345 = VERTEX_POINT ( 'NONE', #9624 ) ;
#2346 = ORIENTED_EDGE ( 'NONE', *, *, #5852, .T. ) ;
#2347 = VERTEX_POINT ( 'NONE', #1373 ) ;
#2348 = DIRECTION ( 'NONE',  ( -1.000000000000000000, 0.000000000000000000, 0.000000000000000000 ) ) ;
#2349 = VERTEX_POINT ( 'NONE', #1222 ) ;
#2350 = ORIENTED_EDGE ( 'NONE', *, *, #10332, .T. ) ;
#2351 = FACE_OUTER_BOUND ( 'NONE', #5450, .T. ) ;
#2352 = DIRECTION ( 'NONE',  ( 1.000000000000000000, 0.000000000000000000, 0.000000000000000000 ) ) ;
#2353 = VERTEX_POINT ( 'NONE', #46 ) ;
#2354 = CARTESIAN_POINT ( 'NONE',  ( -26.45502162804999813, 10.97290950744599947, 60.04999999999999716 ) ) ;
#2355 = DIRECTION ( 'NONE',  ( 0.000000000000000000, 0.000000000000000000, 1.000000000000000000 ) ) ;
#2356 = DIRECTION ( 'NONE',  ( -1.000000000000000000, 0.000000000000000000, 0.000000000000000000 ) ) ;
#2357 = LINE ( 'NONE', #4431, #4938 ) ;
#2358 = DIRECTION ( 'NONE',  ( -0.000000000000000000, -0.000000000000000000, 1.000000000000000000 ) ) ;
#2359 = ORIENTED_EDGE ( 'NONE', *, *, #6536, .T. ) ;
#2360 = ORIENTED_EDGE ( 'NONE', *, *, #8140, .T. ) ;
#2361 = EDGE_CURVE ( 'NONE', #322, #11675, #12888, .T. ) ;
#2362 = ORIENTED_EDGE ( 'NONE', *, *, #816, .F. ) ;
#2363 = EDGE_CURVE ( 'NONE', #9517, #9584, #3821, .T. ) ;
#2364 = DIRECTION ( 'NONE',  ( 0.000000000000000000, 0.000000000000000000, 1.000000000000000000 ) ) ;
#2365 = DIRECTION ( 'NONE',  ( 1.000000000000000000, 0.000000000000000000, 0.000000000000000000 ) ) ;
#2366 = EDGE_CURVE ( 'NONE', #12635, #12583, #2855, .T. ) ;
#2367 = VERTEX_POINT ( 'NONE', #7563 ) ;
#2368 = CARTESIAN_POINT ( 'NONE',  ( -18.05918829504999934, 10.97290950744599947, 118.8499999999999943 ) ) ;
#2369 = FACE_OUTER_BOUND ( 'NONE', #1819, .T. ) ;
#2370 = AXIS2_PLACEMENT_3D ( 'NONE', #6985, #3658, #364 ) ;
#2371 = CARTESIAN_POINT ( 'NONE',  ( -18.97831362643889364, 30.34240036357632775, 53.11745017557792892 ) ) ;
#2372 = CARTESIAN_POINT ( 'NONE',  ( -18.05918829504999934, 10.97290950744599947, 27.09999999999999787 ) ) ;
#2373 = ORIENTED_EDGE ( 'NONE', *, *, #4555, .F. ) ;
#2374 = CARTESIAN_POINT ( 'NONE',  ( -18.05918829504999934, 3.815137874446000055, 61.70038048199999281 ) ) ;
#2375 = DIRECTION ( 'NONE',  ( -0.000000000000000000, -0.000000000000000000, -1.000000000000000000 ) ) ;
#2376 = DIRECTION ( 'NONE',  ( 1.000000000000000000, 0.000000000000000000, 0.000000000000000000 ) ) ;
#2377 = DIRECTION ( 'NONE',  ( 1.000000000000000000, 0.000000000000000000, 0.000000000000000000 ) ) ;
#2378 = ADVANCED_FACE ( 'NONE', ( #10738 ), #7484, .F. ) ;
#2379 = AXIS2_PLACEMENT_3D ( 'NONE', #13326, #13199, #7946 ) ;
#2380 = VERTEX_POINT ( 'NONE', #4381 ) ;
#2381 = ADVANCED_FACE ( 'NONE', ( #11854 ), #2305, .T. ) ;
#2382 = EDGE_LOOP ( 'NONE', ( #7662, #6702 ) ) ;
#2383 = DIRECTION ( 'NONE',  ( 0.000000000000000000, 0.000000000000000000, 1.000000000000000000 ) ) ;
#2384 = VERTEX_POINT ( 'NONE', #10247 ) ;
#2385 = EDGE_CURVE ( 'NONE', #5130, #13231, #387, .T. ) ;
#2386 = ORIENTED_EDGE ( 'NONE', *, *, #1899, .F. ) ;
#2387 = CARTESIAN_POINT ( 'NONE',  ( -43.05918829505002066, 32.97290950744599769, 10.00000000000000000 ) ) ;
#2388 = DIRECTION ( 'NONE',  ( 0.000000000000000000, 0.000000000000000000, 1.000000000000000000 ) ) ;
#2389 = CARTESIAN_POINT ( 'NONE',  ( -3.499999999999998224, 2.499999999999999556, -65.00000000000000000 ) ) ;
#2390 = DIRECTION ( 'NONE',  ( 1.000000000000000000, 0.000000000000000000, 0.000000000000000000 ) ) ;
#2391 = FACE_OUTER_BOUND ( 'NONE', #164, .T. ) ;
#2392 = DIRECTION ( 'NONE',  ( 1.000000000000000000, 0.000000000000000000, 0.000000000000000000 ) ) ;
#2393 = EDGE_CURVE ( 'NONE', #467, #10600, #12519, .T. ) ;
#2394 = CIRCLE ( 'NONE', #7463, 6.000000000000000888 ) ;
#2395 = DIRECTION ( 'NONE',  ( 1.000000000000000000, 0.000000000000000000, 0.000000000000000000 ) ) ;
#2396 = DIRECTION ( 'NONE',  ( -0.000000000000000000, 1.000000000000000000, -0.000000000000000000 ) ) ;
#2397 = ORIENTED_EDGE ( 'NONE', *, *, #1225, .F. ) ;
#2398 = EDGE_CURVE ( 'NONE', #1270, #2036, #530, .T. ) ;
#2399 = CIRCLE ( 'NONE', #7707, 3.000000000000002665 ) ;
#2400 = CARTESIAN_POINT ( 'NONE',  ( -17.52807689001588898, 30.35571874317117036, 53.02236195993357626 ) ) ;
#2401 = VERTEX_POINT ( 'NONE', #13372 ) ;
#2402 = EDGE_LOOP ( 'NONE', ( #7013, #8334, #3909, #6606 ) ) ;
#2403 = CARTESIAN_POINT ( 'NONE',  ( -18.05918829504999934, 10.97290950744599947, 60.40999999999999659 ) ) ;
#2404 = EDGE_CURVE ( 'NONE', #13749, #4490, #13171, .T. ) ;
#2405 = CARTESIAN_POINT ( 'NONE',  ( 0.09777679598749940137, 23.36596564213564875, 68.85549045786049760 ) ) ;
#2406 = DIRECTION ( 'NONE',  ( -1.000000000000000000, 0.000000000000000000, -0.000000000000000000 ) ) ;
#2407 = ORIENTED_EDGE ( 'NONE', *, *, #11274, .T. ) ;
#2408 = LINE ( 'NONE', #1253, #3768 ) ;
#2409 = ADVANCED_FACE ( 'NONE', ( #5828 ), #1437, .T. ) ;
#2410 =( BOUNDED_CURVE ( )  B_SPLINE_CURVE ( 3, ( #5641, #343, #8015, #5847 ),
 .UNSPECIFIED., .F., .F. ) 
 B_SPLINE_CURVE_WITH_KNOTS ( ( 4, 4 ),
 ( 4.712388980384695891, 6.283185307179586232 ),
 .UNSPECIFIED. ) 
 CURVE ( )  GEOMETRIC_REPRESENTATION_ITEM ( )  RATIONAL_B_SPLINE_CURVE ( ( 1.000000000000000000, 0.8047378541243663808, 0.8047378541243663808, 1.000000000000000000 ) ) 
 REPRESENTATION_ITEM ( '' )  );
#2411 = FACE_OUTER_BOUND ( 'NONE', #6638, .T. ) ;
#2412 = AXIS2_PLACEMENT_3D ( 'NONE', #2814, #6906, #13130 ) ;
#2413 = CARTESIAN_POINT ( 'NONE',  ( -15.74360204493244986, 8.348398063716610196, 68.84999999999999432 ) ) ;
#2414 = VERTEX_POINT ( 'NONE', #9047 ) ;
#2415 = EDGE_CURVE ( 'NONE', #6705, #5000, #2646, .T. ) ;
#2416 = CARTESIAN_POINT ( 'NONE',  ( 68.49370948373500312, 113.0390816101113387, 0.000000000000000000 ) ) ;
#2417 = ORIENTED_EDGE ( 'NONE', *, *, #7104, .T. ) ;
#2418 = ORIENTED_EDGE ( 'NONE', *, *, #10599, .F. ) ;
#2419 = VECTOR ( 'NONE', #12619, 1000.000000000000000 ) ;
#2420 = EDGE_LOOP ( 'NONE', ( #7600, #94, #3579, #494 ) ) ;
#2421 = DIRECTION ( 'NONE',  ( 0.000000000000000000, 0.000000000000000000, 1.000000000000000000 ) ) ;
#2422 = CARTESIAN_POINT ( 'NONE',  ( -18.05918829504999934, 28.64232754551664684, 57.35000000000000142 ) ) ;
#2423 = ORIENTED_EDGE ( 'NONE', *, *, #10266, .F. ) ;
#2424 = EDGE_CURVE ( 'NONE', #6052, #13581, #2293, .T. ) ;
#2425 = CARTESIAN_POINT ( 'NONE',  ( 112.1804561881462945, 113.0390816101113387, 20.00000000000000000 ) ) ;
#2426 = CARTESIAN_POINT ( 'NONE',  ( -20.45469220996243820, -1.832421873814833901, -3.000000000000000000 ) ) ;
#2427 = CARTESIAN_POINT ( 'NONE',  ( -34.65718996104999405, 19.27191034044602347, 63.13003331700004850 ) ) ;
#2428 = CARTESIAN_POINT ( 'NONE',  ( -21.79515398487389888, 3.617295300293844829, 63.64999999999999858 ) ) ;
#2429 = CARTESIAN_POINT ( 'NONE',  ( -18.05918829504999934, 10.97290950744599947, 5.250000000000000000 ) ) ;
#2430 = AXIS2_PLACEMENT_3D ( 'NONE', #4097, #9526, #8473 ) ;
#2431 = AXIS2_PLACEMENT_3D ( 'NONE', #5267, #3205, #2154 ) ;
#2432 = VERTEX_POINT ( 'NONE', #3817 ) ;
#2433 = ORIENTED_EDGE ( 'NONE', *, *, #3714, .T. ) ;
#2434 = LINE ( 'NONE', #6741, #13524 ) ;
#2435 = VECTOR ( 'NONE', #2396, 1000.000000000000000 ) ;
#2436 = CYLINDRICAL_SURFACE ( 'NONE', #4341, 2.000000000000001776 ) ;
#2437 = VECTOR ( 'NONE', #11624, 1000.000000000000000 ) ;
#2438 = LINE ( 'NONE', #7967, #6491 ) ;
#2439 = CARTESIAN_POINT ( 'NONE',  ( -1.059188295049996231, -6.027090492554000534, 0.000000000000000000 ) ) ;
#2440 = CIRCLE ( 'NONE', #12010, 1.999999999999994893 ) ;
#2441 = CARTESIAN_POINT ( 'NONE',  ( -20.79267224994196894, 30.19895062614576986, 60.39398676968448854 ) ) ;
#2442 = CARTESIAN_POINT ( 'NONE',  ( -16.08092853089235774, 4.500000000000000000, 7.237812082545092451 ) ) ;
#2443 = VERTEX_POINT ( 'NONE', #3745 ) ;
#2444 = CARTESIAN_POINT ( 'NONE',  ( 50.53208251186094202, 104.0090514096174843, 23.00000000000000000 ) ) ;
#2445 = DIRECTION ( 'NONE',  ( 0.000000000000000000, 0.000000000000000000, -1.000000000000000000 ) ) ;
#2446 = DIRECTION ( 'NONE',  ( 0.000000000000000000, 0.000000000000000000, -1.000000000000000000 ) ) ;
#2447 = DIRECTION ( 'NONE',  ( 0.000000000000000000, 0.000000000000000000, -1.000000000000000000 ) ) ;
#2448 = SHAPE_REPRESENTATION_RELATIONSHIP ( 'NONE' , 'NONE' ,  #5156, #1752 ) ;
#2449 = EDGE_CURVE ( 'NONE', #878, #3128, #7599, .T. ) ;
#2450 = AXIS2_PLACEMENT_3D ( 'NONE', #9885, #8816, #3520 ) ;
#2451 = VECTOR ( 'NONE', #3917, 1000.000000000000114 ) ;
#2452 = VECTOR ( 'NONE', #4836, 1000.000000000000000 ) ;
#2453 = EDGE_LOOP ( 'NONE', ( #5662, #11085, #5895, #12385 ) ) ;
#2454 = CARTESIAN_POINT ( 'NONE',  ( 1.653273178848926867E-15, 8.500000000000000000, 13.50000000000000000 ) ) ;
#2455 = FACE_BOUND ( 'NONE', #2751, .T. ) ;
#2456 = ORIENTED_EDGE ( 'NONE', *, *, #3509, .T. ) ;
#2457 = CARTESIAN_POINT ( 'NONE',  ( 0.000000000000000000, 9.000000000000000000, 0.000000000000000000 ) ) ;
#2458 = FACE_OUTER_BOUND ( 'NONE', #9489, .T. ) ;
#2459 = CARTESIAN_POINT ( 'NONE',  ( -18.05918829504999934, 10.00028003023991907, 62.14999999999999858 ) ) ;
#2460 = FACE_OUTER_BOUND ( 'NONE', #1715, .T. ) ;
#2461 = LINE ( 'NONE', #10891, #12983 ) ;
#2462 = VECTOR ( 'NONE', #11651, 1000.000000000000000 ) ;
#2463 = DIRECTION ( 'NONE',  ( 0.000000000000000000, 0.000000000000000000, 1.000000000000000000 ) ) ;
#2464 = DIRECTION ( 'NONE',  ( 0.000000000000000000, 0.000000000000000000, 1.000000000000000000 ) ) ;
#2465 = AXIS2_PLACEMENT_3D ( 'NONE', #4115, #11576, #6264 ) ;
#2466 = LINE ( 'NONE', #9005, #10134 ) ;
#2467 = CARTESIAN_POINT ( 'NONE',  ( -6.000000000000000888, -12.00000000000000178, 7.000000000000000000 ) ) ;
#2468 = ADVANCED_FACE ( 'NONE', ( #6876 ), #7853, .T. ) ;
#2469 = ORIENTED_EDGE ( 'NONE', *, *, #11241, .F. ) ;
#2470 = DIRECTION ( 'NONE',  ( 0.000000000000000000, 0.000000000000000000, 1.000000000000000000 ) ) ;
#2471 = CIRCLE ( 'NONE', #3800, 0.7499999999999966693 ) ;
#2472 = ORIENTED_EDGE ( 'NONE', *, *, #7416, .T. ) ;
#2473 = DIRECTION ( 'NONE',  ( 0.000000000000000000, 0.000000000000000000, 1.000000000000000000 ) ) ;
#2474 = FILL_AREA_STYLE_COLOUR ( '', #6719 ) ;
#2475 = DIRECTION ( 'NONE',  ( -0.000000000000000000, 1.000000000000000000, -0.000000000000000000 ) ) ;
#2476 = CARTESIAN_POINT ( 'NONE',  ( 50.63563590245420443, 94.90549801902425031, 22.75000000000000000 ) ) ;
#2477 = ADVANCED_FACE ( 'NONE', ( #8072 ), #4858, .T. ) ;
#2478 = DIRECTION ( 'NONE',  ( 1.000000000000000000, 0.000000000000000000, 0.000000000000000000 ) ) ;
#2479 = VECTOR ( 'NONE', #8806, 1000.000000000000000 ) ;
#2480 = AXIS2_PLACEMENT_3D ( 'NONE', #11287, #7151, #12547 ) ;
#2481 = ORIENTED_EDGE ( 'NONE', *, *, #734, .F. ) ;
#2482 = EDGE_CURVE ( 'NONE', #7243, #4278, #12969, .T. ) ;
#2483 = EDGE_LOOP ( 'NONE', ( #2139, #1836, #2147, #5005 ) ) ;
#2484 = CARTESIAN_POINT ( 'NONE',  ( 142.6356359024541973, 111.0390816101113245, 19.25000000000000000 ) ) ;
#2485 = ORIENTED_EDGE ( 'NONE', *, *, #70, .F. ) ;
#2486 = ORIENTED_EDGE ( 'NONE', *, *, #7743, .F. ) ;
#2487 =( BOUNDED_CURVE ( )  B_SPLINE_CURVE ( 3, ( #6116, #13465, #10329, #13393 ),
 .UNSPECIFIED., .F., .F. ) 
 B_SPLINE_CURVE_WITH_KNOTS ( ( 4, 4 ),
 ( 3.141592653589793116, 4.712388980384689674 ),
 .UNSPECIFIED. ) 
 CURVE ( )  GEOMETRIC_REPRESENTATION_ITEM ( )  RATIONAL_B_SPLINE_CURVE ( ( 1.000000000000000000, 0.8047378541243649375, 0.8047378541243649375, 1.000000000000000000 ) ) 
 REPRESENTATION_ITEM ( '' )  );
#2488 = PRODUCT_DEFINITION_SHAPE ( 'NONE', 'NONE',  #13811 ) ;
#2489 = ORIENTED_EDGE ( 'NONE', *, *, #12363, .T. ) ;
#2490 = VECTOR ( 'NONE', #3100, 1000.000000000000000 ) ;
#2491 = VECTOR ( 'NONE', #5037, 1000.000000000000114 ) ;
#2492 = FACE_OUTER_BOUND ( 'NONE', #432, .T. ) ;
#2493 = DIRECTION ( 'NONE',  ( 1.000000000000000000, 0.000000000000000000, 0.000000000000000000 ) ) ;
#2494 = VERTEX_POINT ( 'NONE', #2719 ) ;
#2495 = DIRECTION ( 'NONE',  ( 1.000000000000000000, 0.000000000000000000, 0.000000000000000000 ) ) ;
#2496 = CYLINDRICAL_SURFACE ( 'NONE', #5853, 3.450000000000001510 ) ;
#2497 = DIRECTION ( 'NONE',  ( -0.000000000000000000, 1.000000000000000000, -0.000000000000000000 ) ) ;
#2498 = EDGE_CURVE ( 'NONE', #1128, #11621, #12532, .T. ) ;
#2499 = DIRECTION ( 'NONE',  ( -0.000000000000000000, -0.000000000000000000, -1.000000000000000000 ) ) ;
#2500 = AXIS2_PLACEMENT_3D ( 'NONE', #7654, #6553, #8639 ) ;
#2501 = CIRCLE ( 'NONE', #6038, 23.49999999999999645 ) ;
#2502 = EDGE_CURVE ( 'NONE', #9534, #506, #33, .T. ) ;
#2503 = ORIENTED_EDGE ( 'NONE', *, *, #9444, .F. ) ;
#2504 = DIRECTION ( 'NONE',  ( 0.000000000000000000, 0.000000000000000000, 1.000000000000000000 ) ) ;
#2505 = DIRECTION ( 'NONE',  ( -0.7071067811865489050, -8.659560562354948882E-17, -0.7071067811865460184 ) ) ;
#2506 = CARTESIAN_POINT ( 'NONE',  ( -20.60703947854099027, 30.22015921464618771, 60.59533421581512158 ) ) ;
#2507 = AXIS2_PLACEMENT_3D ( 'NONE', #3650, #1326, #9997 ) ;
#2508 = CIRCLE ( 'NONE', #6274, 0.5000000000000004441 ) ;
#2509 = DIRECTION ( 'NONE',  ( -1.000000000000000000, 0.000000000000000000, 0.000000000000000000 ) ) ;
#2510 = ORIENTED_EDGE ( 'NONE', *, *, #11140, .F. ) ;
#2511 = CARTESIAN_POINT ( 'NONE',  ( -7.999999999999996447, -1.701580061351808733E-15, -65.00000000000000000 ) ) ;
#2512 = VECTOR ( 'NONE', #9194, 1000.000000000000000 ) ;
#2513 = DIRECTION ( 'NONE',  ( 0.000000000000000000, 0.000000000000000000, 1.000000000000000000 ) ) ;
#2514 = DIRECTION ( 'NONE',  ( 0.000000000000000000, 0.000000000000000000, -1.000000000000000000 ) ) ;
#2515 = FACE_BOUND ( 'NONE', #9741, .T. ) ;
#2516 = DIRECTION ( 'NONE',  ( 0.000000000000000000, 0.000000000000000000, 1.000000000000000000 ) ) ;
#2517 = ORIENTED_EDGE ( 'NONE', *, *, #4829, .F. ) ;
#2518 = ORIENTED_EDGE ( 'NONE', *, *, #6001, .T. ) ;
#2519 = EDGE_CURVE ( 'NONE', #11621, #1128, #9631, .T. ) ;
#2520 = VECTOR ( 'NONE', #404, 1000.000000000000000 ) ;
#2521 = ORIENTED_EDGE ( 'NONE', *, *, #5106, .F. ) ;
#2522 = DIRECTION ( 'NONE',  ( -0.000000000000000000, 1.000000000000000000, -0.000000000000000000 ) ) ;
#2523 = LINE ( 'NONE', #4462, #11168 ) ;
#2524 = ORIENTED_EDGE ( 'NONE', *, *, #2165, .T. ) ;
#2525 = ORIENTED_EDGE ( 'NONE', *, *, #7957, .T. ) ;
#2526 = LINE ( 'NONE', #11093, #8476 ) ;
#2527 = LINE ( 'NONE', #10187, #2864 ) ;
#2528 = DIRECTION ( 'NONE',  ( 0.000000000000000000, 0.000000000000000000, 1.000000000000000000 ) ) ;
#2529 = CARTESIAN_POINT ( 'NONE',  ( -40.05918829504999934, -14.02709049255400053, 10.00000000000000000 ) ) ;
#2530 = DIRECTION ( 'NONE',  ( 0.000000000000000000, 0.000000000000000000, 1.000000000000000000 ) ) ;
#2531 = ORIENTED_EDGE ( 'NONE', *, *, #9709, .T. ) ;
#2532 = DIRECTION ( 'NONE',  ( 0.000000000000000000, 1.000000000000000000, 0.000000000000000000 ) ) ;
#2533 = FACE_OUTER_BOUND ( 'NONE', #3068, .T. ) ;
#2534 = DIRECTION ( 'NONE',  ( 0.000000000000000000, 0.000000000000000000, -1.000000000000000000 ) ) ;
#2535 =( GEOMETRIC_REPRESENTATION_CONTEXT ( 3 ) GLOBAL_UNCERTAINTY_ASSIGNED_CONTEXT ( ( #10197 ) ) GLOBAL_UNIT_ASSIGNED_CONTEXT ( ( #3271, #4520, #3618 ) ) REPRESENTATION_CONTEXT ( 'NONE', 'WORKASPACE' ) );
#2536 = CARTESIAN_POINT ( 'NONE',  ( -18.05918829504999934, 10.97290950744599947, 57.54999999999999716 ) ) ;
#2537 = CARTESIAN_POINT ( 'NONE',  ( 68.49370948373500312, 75.03908161011133870, 0.7500000000000006661 ) ) ;
#2538 = ORIENTED_EDGE ( 'NONE', *, *, #7080, .T. ) ;
#2539 =( GEOMETRIC_REPRESENTATION_CONTEXT ( 3 ) GLOBAL_UNCERTAINTY_ASSIGNED_CONTEXT ( ( #3231 ) ) GLOBAL_UNIT_ASSIGNED_CONTEXT ( ( #8984, #5678, #3679 ) ) REPRESENTATION_CONTEXT ( 'NONE', 'WORKASPACE' ) );
#2540 = ORIENTED_EDGE ( 'NONE', *, *, #4860, .F. ) ;
#2541 = CARTESIAN_POINT ( 'NONE',  ( 42.63563590245419732, 111.0390816101113387, 0.7500000000000006661 ) ) ;
#2542 = EDGE_CURVE ( 'NONE', #7101, #12858, #13242, .T. ) ;
#2543 = ADVANCED_FACE ( 'NONE', ( #5682, #11022 ), #9961, .T. ) ;
#2544 = ORIENTED_EDGE ( 'NONE', *, *, #4528, .T. ) ;
#2545 = CARTESIAN_POINT ( 'NONE',  ( -20.45469220996243820, -1.832421873814833901, 0.000000000000000000 ) ) ;
#2546 = CARTESIAN_POINT ( 'NONE',  ( -18.05918829504999934, 10.97290950744599947, 68.84999999999999432 ) ) ;
#2547 = SURFACE_STYLE_FILL_AREA ( #9930 ) ;
#2548 = EDGE_CURVE ( 'NONE', #2899, #1411, #8501, .T. ) ;
#2549 = CYLINDRICAL_SURFACE ( 'NONE', #1774, 16.95000000000000284 ) ;
#2550 = CARTESIAN_POINT ( 'NONE',  ( -18.05918829504999934, 2.673908674445999889, 63.13003331699999876 ) ) ;
#2551 = CARTESIAN_POINT ( 'NONE',  ( -43.05918829505002066, 32.97290950744599769, 10.00000000000000000 ) ) ;
#2552 = AXIS2_PLACEMENT_3D ( 'NONE', #3355, #6488, #62 ) ;
#2553 = VERTEX_POINT ( 'NONE', #11356 ) ;
#2554 = CARTESIAN_POINT ( 'NONE',  ( -21.79515398487389888, 3.617295300293844829, 60.04999999999999716 ) ) ;
#2555 = VERTEX_POINT ( 'NONE', #2080 ) ;
#2556 = EDGE_CURVE ( 'NONE', #7736, #5576, #4070, .T. ) ;
#2557 = ORIENTED_EDGE ( 'NONE', *, *, #7029, .F. ) ;
#2558 = ORIENTED_EDGE ( 'NONE', *, *, #2519, .T. ) ;
#2559 = AXIS2_PLACEMENT_3D ( 'NONE', #11239, #1520, #10131 ) ;
#2560 = EDGE_LOOP ( 'NONE', ( #6168, #873, #5066, #7682 ) ) ;
#2561 = CARTESIAN_POINT ( 'NONE',  ( -32.37473156004999453, 3.815137874445994282, 61.70038048200006386 ) ) ;
#2562 = DIRECTION ( 'NONE',  ( 0.000000000000000000, 0.000000000000000000, 1.000000000000000000 ) ) ;
#2563 = ORIENTED_EDGE ( 'NONE', *, *, #2164, .T. ) ;
#2564 = DIRECTION ( 'NONE',  ( -0.000000000000000000, -0.000000000000000000, -1.000000000000000000 ) ) ;
#2565 = LINE ( 'NONE', #3459, #10125 ) ;
#2566 = DIRECTION ( 'NONE',  ( 0.000000000000000000, 0.000000000000000000, 1.000000000000000000 ) ) ;
#2567 = DIRECTION ( 'NONE',  ( 0.000000000000000000, 0.000000000000000000, -1.000000000000000000 ) ) ;
#2568 = ORIENTED_EDGE ( 'NONE', *, *, #6412, .T. ) ;
#2569 = ORIENTED_EDGE ( 'NONE', *, *, #4407, .T. ) ;
#2570 = ORIENTED_EDGE ( 'NONE', *, *, #6345, .F. ) ;
#2571 = EDGE_CURVE ( 'NONE', #6531, #7944, #13712, .T. ) ;
#2572 = CARTESIAN_POINT ( 'NONE',  ( 3.190811704950004657, 27.97290950744599769, 64.85000000000000853 ) ) ;
#2573 = VERTEX_POINT ( 'NONE', #10581 ) ;
#2574 = SURFACE_STYLE_FILL_AREA ( #13299 ) ;
#2575 = CARTESIAN_POINT ( 'NONE',  ( -21.61797324970345002, 30.08605482698171230, 55.74785149929289219 ) ) ;
#2576 = DIRECTION ( 'NONE',  ( -0.000000000000000000, 1.000000000000000000, -0.000000000000000000 ) ) ;
#2577 = CARTESIAN_POINT ( 'NONE',  ( -18.05918829504999934, 10.97290950744599947, 61.10999999999999943 ) ) ;
#2578 = DIRECTION ( 'NONE',  ( 1.000000000000000000, 0.000000000000000000, -0.000000000000000000 ) ) ;
#2579 = DIRECTION ( 'NONE',  ( -0.000000000000000000, -1.000000000000000000, -0.000000000000000000 ) ) ;
#2580 = ADVANCED_FACE ( 'NONE', ( #7211 ), #12470, .F. ) ;
#2581 = FACE_OUTER_BOUND ( 'NONE', #1851, .T. ) ;
#2582 = ORIENTED_EDGE ( 'NONE', *, *, #12206, .T. ) ;
#2583 = EDGE_LOOP ( 'NONE', ( #3306, #1122, #12219, #10903 ) ) ;
#2584 = ORIENTED_EDGE ( 'NONE', *, *, #7199, .F. ) ;
#2585 = EDGE_CURVE ( 'NONE', #6817, #13266, #4730, .T. ) ;
#2586 = AXIS2_PLACEMENT_3D ( 'NONE', #9879, #302, #11745 ) ;
#2587 = DIRECTION ( 'NONE',  ( 0.2878798879079283446, -0.9576665234506834823, 0.000000000000000000 ) ) ;
#2588 = DIRECTION ( 'NONE',  ( 0.000000000000000000, 0.000000000000000000, -1.000000000000000000 ) ) ;
#2589 = CARTESIAN_POINT ( 'NONE',  ( 0.4408117049500004381, 10.97290950744600124, 14.00000000000000000 ) ) ;
#2590 = CYLINDRICAL_SURFACE ( 'NONE', #11536, 0.9499999999999995115 ) ;
#2591 = FACE_OUTER_BOUND ( 'NONE', #5203, .T. ) ;
#2592 = DIRECTION ( 'NONE',  ( 1.000000000000000000, 0.000000000000000000, 0.000000000000000000 ) ) ;
#2593 = ORIENTED_EDGE ( 'NONE', *, *, #9946, .F. ) ;
#2594 = CARTESIAN_POINT ( 'NONE',  ( 116.7775623211734342, 85.78908161011133870, 20.00000000000000000 ) ) ;
#2595 = CARTESIAN_POINT ( 'NONE',  ( -18.05918829504999934, 10.97290950744599947, 62.14999999999999858 ) ) ;
#2596 = CARTESIAN_POINT ( 'NONE',  ( 50.63563590245420443, 108.9054980190242503, 20.00000000000000000 ) ) ;
#2597 = CARTESIAN_POINT ( 'NONE',  ( 3.690811704950009986, -6.027090492554000534, 64.85000000000000853 ) ) ;
#2598 = EDGE_CURVE ( 'NONE', #9237, #5689, #9402, .T. ) ;
#2599 = DIRECTION ( 'NONE',  ( 0.000000000000000000, 0.000000000000000000, -1.000000000000000000 ) ) ;
#2600 = DIRECTION ( 'NONE',  ( -0.000000000000000000, -0.000000000000000000, -1.000000000000000000 ) ) ;
#2601 = VECTOR ( 'NONE', #971, 1000.000000000000000 ) ;
#2602 = PRODUCT_DEFINITION_SHAPE ( 'NONE', 'NONE',  #2207 ) ;
#2603 = ORIENTED_EDGE ( 'NONE', *, *, #6983, .T. ) ;
#2604 = ORIENTED_EDGE ( 'NONE', *, *, #5041, .T. ) ;
#2605 = CYLINDRICAL_SURFACE ( 'NONE', #11056, 1.725000000000000755 ) ;
#2606 = ORIENTED_EDGE ( 'NONE', *, *, #7448, .F. ) ;
#2607 = CARTESIAN_POINT ( 'NONE',  ( -35.05918829505000645, -6.027090492554000534, 5.250000000000000000 ) ) ;
#2608 = CIRCLE ( 'NONE', #13502, 3.000000000000000000 ) ;
#2609 = DIRECTION ( 'NONE',  ( -0.7071067811865500152, 8.659560562354959975E-17, 0.7071067811865450192 ) ) ;
#2610 = LINE ( 'NONE', #11111, #3616 ) ;
#2611 = CARTESIAN_POINT ( 'NONE',  ( -18.05918829504999934, 10.97290950744599947, 61.10999999999999943 ) ) ;
#2612 = CARTESIAN_POINT ( 'NONE',  ( -18.05918829504999934, 10.97290950744599947, 17.25000000000000000 ) ) ;
#2613 = LINE ( 'NONE', #8110, #5445 ) ;
#2614 = EDGE_CURVE ( 'NONE', #3389, #10398, #11193, .T. ) ;
#2615 = AXIS2_PLACEMENT_3D ( 'NONE', #13023, #2504, #7696 ) ;
#2616 = EDGE_LOOP ( 'NONE', ( #3190, #7711, #8717, #7553, #4509 ) ) ;
#2617 = EDGE_CURVE ( 'NONE', #12491, #3628, #13446, .T. ) ;
#2618 = ORIENTED_EDGE ( 'NONE', *, *, #7381, .T. ) ;
#2619 = EDGE_LOOP ( 'NONE', ( #5617, #11059, #4892, #12617 ) ) ;
#2620 = CARTESIAN_POINT ( 'NONE',  ( -17.14006296349294445, 30.34240036356348824, 61.58254982436883296 ) ) ;
#2621 = AXIS2_PLACEMENT_3D ( 'NONE', #1837, #572, #9896 ) ;
#2622 = ORIENTED_EDGE ( 'NONE', *, *, #2072, .F. ) ;
#2623 = ORIENTED_EDGE ( 'NONE', *, *, #2288, .F. ) ;
#2624 = ORIENTED_EDGE ( 'NONE', *, *, #8194, .F. ) ;
#2625 = ORIENTED_EDGE ( 'NONE', *, *, #2404, .F. ) ;
#2626 = DIRECTION ( 'NONE',  ( 0.000000000000000000, 0.000000000000000000, -1.000000000000000000 ) ) ;
#2627 = CARTESIAN_POINT ( 'NONE',  ( -16.04064420431702942, 4.500000000000000000, -9.307586582922249718 ) ) ;
#2628 = VERTEX_POINT ( 'NONE', #10310 ) ;
#2629 = AXIS2_PLACEMENT_3D ( 'NONE', #7810, #1463, #7037 ) ;
#2630 = DIRECTION ( 'NONE',  ( 1.000000000000000000, 0.000000000000000000, 0.000000000000000000 ) ) ;
#2631 = EDGE_CURVE ( 'NONE', #6077, #10095, #2011, .T. ) ;
#2632 = DIRECTION ( 'NONE',  ( 0.000000000000000000, 0.000000000000000000, 1.000000000000000000 ) ) ;
#2633 = LINE ( 'NONE', #519, #1782 ) ;
#2634 = FACE_OUTER_BOUND ( 'NONE', #376, .T. ) ;
#2635 = EDGE_CURVE ( 'NONE', #3128, #1998, #7368, .T. ) ;
#2636 = VERTEX_POINT ( 'NONE', #1861 ) ;
#2637 =( GEOMETRIC_REPRESENTATION_CONTEXT ( 3 ) GLOBAL_UNCERTAINTY_ASSIGNED_CONTEXT ( ( #8094 ) ) GLOBAL_UNIT_ASSIGNED_CONTEXT ( ( #538, #4800, #5634 ) ) REPRESENTATION_CONTEXT ( 'NONE', 'WORKASPACE' ) );
#2638 = ORIENTED_EDGE ( 'NONE', *, *, #6634, .F. ) ;
#2639 = DIRECTION ( 'NONE',  ( 0.000000000000000000, 0.000000000000000000, -1.000000000000000000 ) ) ;
#2640 = DIRECTION ( 'NONE',  ( -0.000000000000000000, -0.000000000000000000, -1.000000000000000000 ) ) ;
#2641 = CARTESIAN_POINT ( 'NONE',  ( -21.45399636639216467, 30.11090903168091870, 59.35894009006398875 ) ) ;
#2642 = ORIENTED_EDGE ( 'NONE', *, *, #1410, .T. ) ;
#2643 = FILL_AREA_STYLE ('',( #10038 ) ) ;
#2644 = DIRECTION ( 'NONE',  ( 0.000000000000000000, 0.000000000000000000, -1.000000000000000000 ) ) ;
#2645 = DIRECTION ( 'NONE',  ( -0.000000000000000000, 1.000000000000000000, -0.000000000000000000 ) ) ;
#2646 = LINE ( 'NONE', #3622, #2951 ) ;
#2647 = AXIS2_PLACEMENT_3D ( 'NONE', #5748, #13093, #8982 ) ;
#2648 = DIRECTION ( 'NONE',  ( 0.000000000000000000, 0.000000000000000000, -1.000000000000000000 ) ) ;
#2649 = EDGE_LOOP ( 'NONE', ( #4958, #10882, #10234, #7832 ) ) ;
#2650 = ADVANCED_FACE ( 'NONE', ( #6098 ), #10371, .F. ) ;
#2651 = AXIS2_PLACEMENT_3D ( 'NONE', #11554, #6242, #9600 ) ;
#2652 = CIRCLE ( 'NONE', #3301, 6.449999999999997513 ) ;
#2653 = VERTEX_POINT ( 'NONE', #869 ) ;
#2654 = AXIS2_PLACEMENT_3D ( 'NONE', #9886, #440, #8968 ) ;
#2655 = ADVANCED_FACE ( 'NONE', ( #796 ), #488, .F. ) ;
#2656 = DIRECTION ( 'NONE',  ( -0.000000000000000000, -0.000000000000000000, -1.000000000000000000 ) ) ;
#2657 = DIRECTION ( 'NONE',  ( 1.000000000000000000, 0.000000000000000000, 0.000000000000000000 ) ) ;
#2658 = LINE ( 'NONE', #1799, #224 ) ;
#2659 = FACE_OUTER_BOUND ( 'NONE', #11248, .T. ) ;
#2660 = DIRECTION ( 'NONE',  ( -0.4528443260392610026, -0.8915896008669278450, 0.000000000000000000 ) ) ;
#2661 = DIRECTION ( 'NONE',  ( 0.000000000000000000, 0.000000000000000000, -1.000000000000000000 ) ) ;
#2662 = FACE_BOUND ( 'NONE', #10571, .T. ) ;
#2663 = DIRECTION ( 'NONE',  ( 1.000000000000000000, 0.000000000000000000, 0.000000000000000000 ) ) ;
#2664 = FACE_OUTER_BOUND ( 'NONE', #3235, .T. ) ;
#2665 = DIRECTION ( 'NONE',  ( 0.6615960714621567096, -0.7498604124941127269, 0.000000000000000000 ) ) ;
#2666 = DIRECTION ( 'NONE',  ( 0.000000000000000000, 0.000000000000000000, 1.000000000000000000 ) ) ;
#2667 = DIRECTION ( 'NONE',  ( 0.000000000000000000, -0.000000000000000000, 1.000000000000000000 ) ) ;
#2668 = CIRCLE ( 'NONE', #7292, 24.92993838181874722 ) ;
#2669 = CIRCLE ( 'NONE', #4663, 2.999999999999999112 ) ;
#2670 = AXIS2_PLACEMENT_3D ( 'NONE', #2324, #4467, #10611 ) ;
#2671 = ADVANCED_FACE ( 'NONE', ( #10516 ), #4027, .F. ) ;
#2672 = VECTOR ( 'NONE', #3884, 1000.000000000000000 ) ;
#2673 = ADVANCED_FACE ( 'NONE', ( #946 ), #8277, .T. ) ;
#2674 = CARTESIAN_POINT ( 'NONE',  ( -24.37001676333060018, -4.028726038184999858, 62.14999999999999858 ) ) ;
#2675 = VECTOR ( 'NONE', #11102, 1000.000000000000000 ) ;
#2676 = CIRCLE ( 'NONE', #11361, 2.000000000000001776 ) ;
#2677 = AXIS2_PLACEMENT_3D ( 'NONE', #10326, #748, #9275 ) ;
#2678 = CARTESIAN_POINT ( 'NONE',  ( -16.55918829504999579, 27.19822998463810393, 57.14449823292466135 ) ) ;
#2679 = AXIS2_PLACEMENT_3D ( 'NONE', #3104, #10627, #4211 ) ;
#2680 = LINE ( 'NONE', #7039, #1565 ) ;
#2681 = CARTESIAN_POINT ( 'NONE',  ( 140.3249757306743675, 112.2890816101113387, 20.00000000000000000 ) ) ;
#2682 = DIRECTION ( 'NONE',  ( 0.000000000000000000, 0.000000000000000000, 1.000000000000000000 ) ) ;
#2683 = DIRECTION ( 'NONE',  ( 0.000000000000000000, 0.000000000000000000, -1.000000000000000000 ) ) ;
#2684 = DIRECTION ( 'NONE',  ( 0.000000000000000000, 0.000000000000000000, -1.000000000000000000 ) ) ;
#2685 = CARTESIAN_POINT ( 'NONE',  ( -18.05918829504999934, 10.97290950744599947, 62.14999999999999858 ) ) ;
#2686 =( GEOMETRIC_REPRESENTATION_CONTEXT ( 3 ) GLOBAL_UNCERTAINTY_ASSIGNED_CONTEXT ( ( #3908 ) ) GLOBAL_UNIT_ASSIGNED_CONTEXT ( ( #4660, #4526, #5830 ) ) REPRESENTATION_CONTEXT ( 'NONE', 'WORKASPACE' ) );
#2687 = AXIS2_PLACEMENT_3D ( 'NONE', #8663, #7521, #3242 ) ;
#2688 = ORIENTED_EDGE ( 'NONE', *, *, #13210, .T. ) ;
#2689 = VECTOR ( 'NONE', #6333, 1000.000000000000000 ) ;
#2690 = ORIENTED_EDGE ( 'NONE', *, *, #10147, .T. ) ;
#2691 =( BOUNDED_CURVE ( )  B_SPLINE_CURVE ( 3, ( #8360, #12692, #9210, #3073 ),
 .UNSPECIFIED., .F., .F. ) 
 B_SPLINE_CURVE_WITH_KNOTS ( ( 4, 4 ),
 ( 1.570796326794896558, 3.141592653589793116 ),
 .UNSPECIFIED. ) 
 CURVE ( )  GEOMETRIC_REPRESENTATION_ITEM ( )  RATIONAL_B_SPLINE_CURVE ( ( 1.000000000000000000, 0.8047378541243649375, 0.8047378541243649375, 1.000000000000000000 ) ) 
 REPRESENTATION_ITEM ( '' )  );
#2692 = ORIENTED_EDGE ( 'NONE', *, *, #11226, .F. ) ;
#2693 = CARTESIAN_POINT ( 'NONE',  ( -16.76337124042152382, 30.32416700402973575, 61.44969122351110968 ) ) ;
#2694 = ORIENTED_EDGE ( 'NONE', *, *, #5908, .T. ) ;
#2695 = EDGE_LOOP ( 'NONE', ( #6955, #7533 ) ) ;
#2696 = DIRECTION ( 'NONE',  ( 0.6615960714621565986, -0.7498604124941126159, 0.000000000000000000 ) ) ;
#2697 = VERTEX_POINT ( 'NONE', #3127 ) ;
#2698 = PLANE ( 'NONE',  #8711 ) ;
#2699 = PLANE ( 'NONE',  #13563 ) ;
#2700 = EDGE_CURVE ( 'NONE', #1551, #51, #1371, .T. ) ;
#2701 = PLANE ( 'NONE',  #11792 ) ;
#2702 = ORIENTED_EDGE ( 'NONE', *, *, #7155, .F. ) ;
#2703 = LINE ( 'NONE', #8756, #6946 ) ;
#2704 = AXIS2_PLACEMENT_3D ( 'NONE', #563, #9873, #4822 ) ;
#2705 = VECTOR ( 'NONE', #13244, 1000.000000000000000 ) ;
#2706 = DIRECTION ( 'NONE',  ( -1.000000000000000000, 0.000000000000000000, 0.000000000000000000 ) ) ;
#2707 = ORIENTED_EDGE ( 'NONE', *, *, #4060, .T. ) ;
#2708 = VECTOR ( 'NONE', #2263, 1000.000000000000000 ) ;
#2709 = ORIENTED_EDGE ( 'NONE', *, *, #7319, .T. ) ;
#2710 = DIRECTION ( 'NONE',  ( 0.000000000000000000, 0.000000000000000000, 1.000000000000000000 ) ) ;
#2711 = VERTEX_POINT ( 'NONE', #7545 ) ;
#2712 = EDGE_CURVE ( 'NONE', #11467, #878, #12318, .T. ) ;
#2713 = ORIENTED_EDGE ( 'NONE', *, *, #6399, .F. ) ;
#2714 = EDGE_CURVE ( 'NONE', #9883, #6370, #9185, .T. ) ;
#2715 = DIRECTION ( 'NONE',  ( 0.000000000000000000, 0.000000000000000000, 1.000000000000000000 ) ) ;
#2716 = CARTESIAN_POINT ( 'NONE',  ( -20.96223510382219857, 30.17819129720234628, 60.18295065293622059 ) ) ;
#2717 = LINE ( 'NONE', #11284, #6753 ) ;
#2718 = LINE ( 'NONE', #7210, #166 ) ;
#2719 = CARTESIAN_POINT ( 'NONE',  ( -1.059188295050000894, 10.97290950744599947, 14.00000000000000000 ) ) ;
#2720 = CARTESIAN_POINT ( 'NONE',  ( -25.86749127492454647, -8.860076549334127805, 5.250000000000000000 ) ) ;
#2721 = CIRCLE ( 'NONE', #4052, 4.750000000000000888 ) ;
#2722 = VECTOR ( 'NONE', #2661, 1000.000000000000000 ) ;
#2723 = CARTESIAN_POINT ( 'NONE',  ( -82.05918829505003487, 0.000000000000000000, 70.79081170495001629 ) ) ;
#2724 = VECTOR ( 'NONE', #6307, 1000.000000000000000 ) ;
#2725 = VECTOR ( 'NONE', #6013, 1000.000000000000000 ) ;
#2726 = AXIS2_PLACEMENT_3D ( 'NONE', #2960, #13539, #6975 ) ;
#2727 = CARTESIAN_POINT ( 'NONE',  ( -38.38077571930826082, -0.4981161769137699147, 17.25000000000000000 ) ) ;
#2728 = CARTESIAN_POINT ( 'NONE',  ( -18.05918829504999934, 10.97290950744599947, 63.54999999999999716 ) ) ;
#2729 = AXIS2_PLACEMENT_3D ( 'NONE', #10537, #6340, #964 ) ;
#2730 = VERTEX_POINT ( 'NONE', #1274 ) ;
#2731 = CARTESIAN_POINT ( 'NONE',  ( -20.77625425128555392, 5.623371902244430842, 60.04999999999999716 ) ) ;
#2732 = EDGE_CURVE ( 'NONE', #10905, #3167, #13196, .T. ) ;
#2733 = CARTESIAN_POINT ( 'NONE',  ( 0.000000000000000000, 0.000000000000000000, 0.000000000000000000 ) ) ;
#2734 = CYLINDRICAL_SURFACE ( 'NONE', #1067, 1.999999999999994893 ) ;
#2735 = CARTESIAN_POINT ( 'NONE',  ( -35.05918829505000645, 27.97290950744599769, 64.85000000000000853 ) ) ;
#2736 = CARTESIAN_POINT ( 'NONE',  ( -21.78591716150126700, 14.35275298274230771, 68.85000000000003695 ) ) ;
#2737 = LINE ( 'NONE', #4745, #8002 ) ;
#2738 = CYLINDRICAL_SURFACE ( 'NONE', #5530, 0.2500000000000002220 ) ;
#2739 = CARTESIAN_POINT ( 'NONE',  ( 1.940811704950003991, 27.97290950744599769, 10.00000000000000000 ) ) ;
#2740 = DIRECTION ( 'NONE',  ( -1.000000000000000000, 0.000000000000000000, 0.000000000000000000 ) ) ;
#2741 = CARTESIAN_POINT ( 'NONE',  ( 12.00000000000000000, 2.500000000000000000, 0.000000000000000000 ) ) ;
#2742 = ADVANCED_FACE ( 'NONE', ( #9816 ), #1070, .T. ) ;
#2743 = VECTOR ( 'NONE', #12842, 1000.000000000000114 ) ;
#2744 = AXIS2_PLACEMENT_3D ( 'NONE', #5604, #311, #4501 ) ;
#2745 = AXIS2_PLACEMENT_3D ( 'NONE', #1925, #10438, #7075 ) ;
#2746 = VERTEX_POINT ( 'NONE', #4304 ) ;
#2747 = ORIENTED_EDGE ( 'NONE', *, *, #9742, .T. ) ;
#2748 = VERTEX_POINT ( 'NONE', #4232 ) ;
#2749 = DIRECTION ( 'NONE',  ( -1.000000000000000000, 0.000000000000000000, 0.000000000000000000 ) ) ;
#2750 = ORIENTED_EDGE ( 'NONE', *, *, #3059, .F. ) ;
#2752 = EDGE_CURVE ( 'NONE', #1026, #5173, #268, .T. ) ;
#2751 = EDGE_LOOP ( 'NONE', ( #1166, #11731 ) ) ;
#2753 = FACE_OUTER_BOUND ( 'NONE', #774, .T. ) ;
#2754 = CIRCLE ( 'NONE', #4513, 2.500000000000000000 ) ;
#2755 = CARTESIAN_POINT ( 'NONE',  ( -18.05918829504999934, 10.97290950744599947, 60.65000000000000568 ) ) ;
#2756 =( NAMED_UNIT ( * ) PLANE_ANGLE_UNIT ( ) SI_UNIT ( $, .RADIAN. ) );
#2757 = DIRECTION ( 'NONE',  ( 0.000000000000000000, 1.000000000000000000, 0.000000000000000000 ) ) ;
#2758 = DIRECTION ( 'NONE',  ( 0.000000000000000000, 0.000000000000000000, -1.000000000000000000 ) ) ;
#2759 = DIRECTION ( 'NONE',  ( 0.000000000000000000, 0.000000000000000000, -1.000000000000000000 ) ) ;
#2760 = EDGE_CURVE ( 'NONE', #5663, #5817, #2066, .T. ) ;
#2761 = DIRECTION ( 'NONE',  ( 1.000000000000000000, 0.000000000000000000, 0.000000000000000000 ) ) ;
#2762 = AXIS2_PLACEMENT_3D ( 'NONE', #7423, #6466, #10733 ) ;
#2763 = VERTEX_POINT ( 'NONE', #7467 ) ;
#2764 = LINE ( 'NONE', #434, #13713 ) ;
#2765 = ORIENTED_EDGE ( 'NONE', *, *, #11415, .T. ) ;
#2766 = EDGE_LOOP ( 'NONE', ( #9909, #7352, #13693, #5713, #2359, #9445, #4998, #6703, #10631, #832, #13574, #7415, #7002, #6417, #2882 ) ) ;
#2767 = DIRECTION ( 'NONE',  ( -1.182766006347823109E-16, 1.000000000000000000, -0.000000000000000000 ) ) ;
#2768 = ORIENTED_EDGE ( 'NONE', *, *, #469, .T. ) ;
#2769 = FACE_BOUND ( 'NONE', #3364, .T. ) ;
#2770 = DIRECTION ( 'NONE',  ( 0.000000000000000000, -1.000000000000000000, 0.000000000000000000 ) ) ;
#2771 = CARTESIAN_POINT ( 'NONE',  ( 134.6356359024541973, 89.90549801902423610, 22.75000000000000000 ) ) ;
#2772 = ORIENTED_EDGE ( 'NONE', *, *, #10363, .F. ) ;
#2773 = DIRECTION ( 'NONE',  ( 0.000000000000000000, 1.000000000000000000, -0.000000000000000000 ) ) ;
#2774 = VECTOR ( 'NONE', #1066, 1000.000000000000000 ) ;
#2775 = DIRECTION ( 'NONE',  ( 1.000000000000000000, 0.000000000000000000, 0.000000000000000000 ) ) ;
#2776 = DIRECTION ( 'NONE',  ( 1.000000000000000000, 0.000000000000000000, 0.000000000000000000 ) ) ;
#2777 = EDGE_CURVE ( 'NONE', #11352, #5468, #2357, .T. ) ;
#2778 = CARTESIAN_POINT ( 'NONE',  ( -18.05918829504999934, 10.97290950744599947, 64.54999999999999716 ) ) ;
#2779 = VERTEX_POINT ( 'NONE', #11758 ) ;
#2780 = CIRCLE ( 'NONE', #9454, 4.750000000000000000 ) ;
#2781 = VERTEX_POINT ( 'NONE', #5326 ) ;
#2782 = ORIENTED_EDGE ( 'NONE', *, *, #1866, .T. ) ;
#2783 = ORIENTED_EDGE ( 'NONE', *, *, #2795, .F. ) ;
#2784 = EDGE_LOOP ( 'NONE', ( #4148, #7186, #11195, #9958, #2179 ) ) ;
#2785 = DIRECTION ( 'NONE',  ( -0.000000000000000000, 1.000000000000000000, -0.000000000000000000 ) ) ;
#2786 = CARTESIAN_POINT ( 'NONE',  ( 84.99521369064696330, 82.14063840035363739, 10.00000000000000000 ) ) ;
#2787 = DIRECTION ( 'NONE',  ( 0.000000000000000000, 0.000000000000000000, 1.000000000000000000 ) ) ;
#2788 = CARTESIAN_POINT ( 'NONE',  ( -35.05918829505000645, -6.027090492554000534, 64.35000000000000853 ) ) ;
#2789 = DIRECTION ( 'NONE',  ( 0.6615960714621568206, -0.7498604124941125049, 0.000000000000000000 ) ) ;
#2790 = FACE_OUTER_BOUND ( 'NONE', #6814, .T. ) ;
#2791 = ORIENTED_EDGE ( 'NONE', *, *, #4555, .T. ) ;
#2792 = VECTOR ( 'NONE', #11678, 1000.000000000000000 ) ;
#2793 = ADVANCED_FACE ( 'NONE', ( #8686 ), #11832, .T. ) ;
#2794 = ADVANCED_FACE ( 'NONE', ( #6654 ), #7686, .F. ) ;
#2795 = EDGE_CURVE ( 'NONE', #10214, #13286, #12082, .T. ) ;
#2796 = CARTESIAN_POINT ( 'NONE',  ( -24.35918829505000005, 10.97290950744599947, 63.02000000000000313 ) ) ;
#2797 = CARTESIAN_POINT ( 'NONE',  ( 12.81426999815521839, -15.06602133594279991, 7.000000000000000000 ) ) ;
#2798 = EDGE_LOOP ( 'NONE', ( #8036, #5301, #3189, #9082 ) ) ;
#2799 = DIRECTION ( 'NONE',  ( -1.000000000000000000, 0.000000000000000000, 0.000000000000000000 ) ) ;
#2800 = CARTESIAN_POINT ( 'NONE',  ( 140.6356359024541689, 85.03908161011133870, 19.25000000000000000 ) ) ;
#2801 = CARTESIAN_POINT ( 'NONE',  ( -30.32854245105399826, 27.54455229823479812, 68.85549045786049760 ) ) ;
#2802 = LINE ( 'NONE', #6959, #5814 ) ;
#2803 = CARTESIAN_POINT ( 'NONE',  ( 81.82136590429890077, 114.1051029460540605, 10.00000000000000000 ) ) ;
#2804 = DIRECTION ( 'NONE',  ( 0.000000000000000000, 0.000000000000000000, 1.000000000000000000 ) ) ;
#2805 = CARTESIAN_POINT ( 'NONE',  ( 50.63563590245420443, 108.6554980190242503, 22.75000000000000000 ) ) ;
#2806 = FACE_OUTER_BOUND ( 'NONE', #2117, .T. ) ;
#2807 = CARTESIAN_POINT ( 'NONE',  ( 140.5320825118609207, 108.8019446284309737, 23.00000000000000000 ) ) ;
#2808 = FACE_OUTER_BOUND ( 'NONE', #7830, .T. ) ;
#2809 = EDGE_CURVE ( 'NONE', #3595, #6971, #12747, .T. ) ;
#2810 = ORIENTED_EDGE ( 'NONE', *, *, #10201, .T. ) ;
#2811 = LINE ( 'NONE', #897, #568 ) ;
#2812 = CLOSED_SHELL ( 'NONE', ( #13467, #5366, #833, #3183, #11924, #11985, #1267, #11129, #12404, #9536, #3247, #9036, #2842, #12521, #10500, #11684, #8483, #10388, #3757, #8654, #2922, #12950, #8702, #5981, #5775, #3924, #6119, #297, #2886, #6063, #3501, #1681, #3918 ) ) ;
#2813 = EDGE_LOOP ( 'NONE', ( #2313, #4007, #10116, #12536 ) ) ;
#2814 = CARTESIAN_POINT ( 'NONE',  ( -35.05918829505000645, -6.027090492554000534, 68.85549045786049760 ) ) ;
#2815 = CARTESIAN_POINT ( 'NONE',  ( 140.6356359024541973, 85.03908161011132449, 0.3106601717798216367 ) ) ;
#2816 = EDGE_CURVE ( 'NONE', #8976, #10798, #4504, .T. ) ;
#2817 =( NAMED_UNIT ( * ) PLANE_ANGLE_UNIT ( ) SI_UNIT ( $, .RADIAN. ) );
#2818 = CARTESIAN_POINT ( 'NONE',  ( 92.63563590245421153, 99.03908161011133870, 20.00000000000000000 ) ) ;
#2819 = VECTOR ( 'NONE', #10921, 1000.000000000000000 ) ;
#2820 = CARTESIAN_POINT ( 'NONE',  ( -18.05918829504999223, 2.660265422445993622, 63.26601075299999621 ) ) ;
#2821 = CARTESIAN_POINT ( 'NONE',  ( -18.05918829504999934, 10.97290950744599947, 61.65955166399999854 ) ) ;
#2822 = DIRECTION ( 'NONE',  ( 0.000000000000000000, 0.000000000000000000, 1.000000000000000000 ) ) ;
#2823 = EDGE_CURVE ( 'NONE', #2711, #13343, #5330, .T. ) ;
#2824 = ORIENTED_EDGE ( 'NONE', *, *, #8285, .T. ) ;
#2825 = CIRCLE ( 'NONE', #5912, 17.00000000000000000 ) ;
#2826 = VERTEX_POINT ( 'NONE', #2428 ) ;
#2827 = CARTESIAN_POINT ( 'NONE',  ( -14.81288417521985856, 30.13232420324952443, 55.04779169721881971 ) ) ;
#2828 = ORIENTED_EDGE ( 'NONE', *, *, #112, .F. ) ;
#2829 = EDGE_CURVE ( 'NONE', #1279, #7735, #1559, .T. ) ;
#2830 = FACE_OUTER_BOUND ( 'NONE', #26, .T. ) ;
#2831 = DIRECTION ( 'NONE',  ( 0.000000000000000000, 0.000000000000000000, 1.000000000000000000 ) ) ;
#2832 = EDGE_LOOP ( 'NONE', ( #10672, #4684, #5805, #8541 ) ) ;
#2833 = EDGE_LOOP ( 'NONE', ( #5875, #6796, #5453, #10803, #2104, #8113 ) ) ;
#2834 = DIRECTION ( 'NONE',  ( 1.000000000000000000, 0.000000000000000000, 0.000000000000000000 ) ) ;
#2835 = DIRECTION ( 'NONE',  ( 0.000000000000000000, 1.000000000000000000, 0.000000000000000000 ) ) ;
#2836 = VERTEX_POINT ( 'NONE', #11699 ) ;
#2837 = DIRECTION ( 'NONE',  ( -0.000000000000000000, 1.000000000000000000, -0.000000000000000000 ) ) ;
#2838 = CARTESIAN_POINT ( 'NONE',  ( -16.04064420431702942, 4.500000000000000000, -9.307586582922249718 ) ) ;
#2839 = CARTESIAN_POINT ( 'NONE',  ( -22.71804201037815218, -4.525318844826149878, 63.45000000000000284 ) ) ;
#2840 = AXIS2_PLACEMENT_3D ( 'NONE', #3895, #664, #6172 ) ;
#2841 = DIRECTION ( 'NONE',  ( 0.000000000000000000, -1.000000000000000000, 0.000000000000000000 ) ) ;
#2842 = ADVANCED_FACE ( 'NONE', ( #2287 ), #2143, .F. ) ;
#2843 = ADVANCED_FACE ( 'NONE', ( #92 ), #7113, .F. ) ;
#2844 = ORIENTED_EDGE ( 'NONE', *, *, #6030, .F. ) ;
#2845 = EDGE_LOOP ( 'NONE', ( #452, #11261 ) ) ;
#2846 = AXIS2_PLACEMENT_3D ( 'NONE', #3, #3292, #3439 ) ;
#2847 = ADVANCED_FACE ( 'NONE', ( #3670 ), #10021, .F. ) ;
#2848 = ORIENTED_EDGE ( 'NONE', *, *, #6277, .F. ) ;
#2849 = LINE ( 'NONE', #3812, #12228 ) ;
#2850 = CARTESIAN_POINT ( 'NONE',  ( -20.28307750662727571, 30.25357667928725647, 60.89116620645845046 ) ) ;
#2851 = CARTESIAN_POINT ( 'NONE',  ( 0.000000000000000000, 0.000000000000000000, 7.000000000000000000 ) ) ;
#2852 = DIRECTION ( 'NONE',  ( 0.000000000000000000, 0.000000000000000000, 1.000000000000000000 ) ) ;
#2853 = DIRECTION ( 'NONE',  ( 1.000000000000000000, 0.000000000000000000, 0.000000000000000000 ) ) ;
#2854 = DIRECTION ( 'NONE',  ( 0.000000000000000000, 0.000000000000000000, 1.000000000000000000 ) ) ;
#2855 =( BOUNDED_CURVE ( )  B_SPLINE_CURVE ( 3, ( #10810, #4584, #7427, #6470 ),
 .UNSPECIFIED., .F., .F. ) 
 B_SPLINE_CURVE_WITH_KNOTS ( ( 4, 4 ),
 ( 0.04873315200000220143, 0.9512668486397960477 ),
 .UNSPECIFIED. ) 
 CURVE ( )  GEOMETRIC_REPRESENTATION_ITEM ( )  RATIONAL_B_SPLINE_CURVE ( ( 0.9230982619916300314, 0.4726811438562560364, 0.4726811441755530141, 0.9230982629495190217 ) ) 
 REPRESENTATION_ITEM ( '' )  );
#2856 = DIRECTION ( 'NONE',  ( 1.000000000000000000, 0.000000000000000000, 0.000000000000000000 ) ) ;
#2857 = ORIENTED_EDGE ( 'NONE', *, *, #2393, .F. ) ;
#2858 = VERTEX_POINT ( 'NONE', #5668 ) ;
#2859 = CARTESIAN_POINT ( 'NONE',  ( -25.32001676333059947, -4.028726038184999858, 62.14999999999999858 ) ) ;
#2860 = CARTESIAN_POINT ( 'NONE',  ( 50.63563590245420443, 89.90549801902423610, 22.75000000000000000 ) ) ;
#2861 = ORIENTED_EDGE ( 'NONE', *, *, #6604, .T. ) ;
#2862 = DIRECTION ( 'NONE',  ( 0.4528443260392608916, 0.8915896008669279560, 0.000000000000000000 ) ) ;
#2863 = DIRECTION ( 'NONE',  ( -0.4528443260392611136, -0.8915896008669277339, 0.000000000000000000 ) ) ;
#2864 = VECTOR ( 'NONE', #604, 1000.000000000000000 ) ;
#2865 = FACE_OUTER_BOUND ( 'NONE', #9805, .T. ) ;
#2866 = CARTESIAN_POINT ( 'NONE',  ( -6.000000000000000888, 11.99999999999999822, 7.000000000000000000 ) ) ;
#2867 = CARTESIAN_POINT ( 'NONE',  ( -21.36716865236079954, 14.72221156991656166, 68.84999999999999432 ) ) ;
#2868 = DIRECTION ( 'NONE',  ( 0.000000000000000000, 0.000000000000000000, 1.000000000000000000 ) ) ;
#2869 = EDGE_CURVE ( 'NONE', #12554, #525, #2633, .T. ) ;
#2870 = LINE ( 'NONE', #11371, #9408 ) ;
#2871 = FACE_OUTER_BOUND ( 'NONE', #4641, .T. ) ;
#2872 = AXIS2_PLACEMENT_3D ( 'NONE', #4523, #12400, #11424 ) ;
#2873 = AXIS2_PLACEMENT_3D ( 'NONE', #12688, #10871, #1152 ) ;
#2874 = EDGE_LOOP ( 'NONE', ( #11378, #9881, #10391, #9389 ) ) ;
#2875 = DIRECTION ( 'NONE',  ( 0.000000000000000000, 0.000000000000000000, 1.000000000000000000 ) ) ;
#2876 = VERTEX_POINT ( 'NONE', #13155 ) ;
#2877 = ORIENTED_EDGE ( 'NONE', *, *, #1052, .F. ) ;
#2878 = DIRECTION ( 'NONE',  ( 1.000000000000000000, 0.000000000000000000, 0.000000000000000000 ) ) ;
#2879 = LINE ( 'NONE', #13538, #11401 ) ;
#2880 = AXIS2_PLACEMENT_3D ( 'NONE', #6978, #7685, #4503 ) ;
#2881 = SURFACE_STYLE_FILL_AREA ( #13409 ) ;
#2882 = ORIENTED_EDGE ( 'NONE', *, *, #8783, .T. ) ;
#2883 = CIRCLE ( 'NONE', #12880, 6.000000000000002665 ) ;
#2884 = CONICAL_SURFACE ( 'NONE', #8882, 4.250000000000000000, 0.7853981633974524978 ) ;
#2885 = CARTESIAN_POINT ( 'NONE',  ( -24.65502162805000097, 10.97290950744599947, 60.40999999999999659 ) ) ;
#2886 = ADVANCED_FACE ( 'NONE', ( #3604 ), #1562, .F. ) ;
#2887 = AXIS2_PLACEMENT_3D ( 'NONE', #7900, #13285, #5523 ) ;
#2888 = DIRECTION ( 'NONE',  ( 0.000000000000000000, 0.000000000000000000, 1.000000000000000000 ) ) ;
#2889 = FACE_OUTER_BOUND ( 'NONE', #4688, .T. ) ;
#2890 = ADVANCED_FACE ( 'NONE', ( #6793 ), #8897, .T. ) ;
#2891 =( GEOMETRIC_REPRESENTATION_CONTEXT ( 3 ) GLOBAL_UNCERTAINTY_ASSIGNED_CONTEXT ( ( #11307 ) ) GLOBAL_UNIT_ASSIGNED_CONTEXT ( ( #109, #4323, #11084 ) ) REPRESENTATION_CONTEXT ( 'NONE', 'WORKASPACE' ) );
#2892 = EDGE_CURVE ( 'NONE', #1270, #8617, #12251, .T. ) ;
#2893 = AXIS2_PLACEMENT_3D ( 'NONE', #7680, #9730, #11964 ) ;
#2894 = VECTOR ( 'NONE', #9046, 1000.000000000000000 ) ;
#2895 = EDGE_LOOP ( 'NONE', ( #6624, #15, #4647, #4108 ) ) ;
#2896 = AXIS2_PLACEMENT_3D ( 'NONE', #5772, #1451, #3762 ) ;
#2897 = EDGE_LOOP ( 'NONE', ( #9668, #4967, #1209, #7175 ) ) ;
#2898 = CARTESIAN_POINT ( 'NONE',  ( -14.57973916105114753, 30.09823897628803024, 59.16325671210135795 ) ) ;
#2899 = VERTEX_POINT ( 'NONE', #5811 ) ;
#2900 = VERTEX_POINT ( 'NONE', #4781 ) ;
#2901 = LINE ( 'NONE', #7698, #1619 ) ;
#2902 =( REPRESENTATION_RELATIONSHIP ('NONE','NONE', #11848, #13195 ) REPRESENTATION_RELATIONSHIP_WITH_TRANSFORMATION ( #6527 )SHAPE_REPRESENTATION_RELATIONSHIP( ) );
#2903 = DIRECTION ( 'NONE',  ( 0.000000000000000000, 0.000000000000000000, -1.000000000000000000 ) ) ;
#2904 = CYLINDRICAL_SURFACE ( 'NONE', #9563, 0.5000000000000004441 ) ;
#2905 = LINE ( 'NONE', #8255, #2452 ) ;
#2906 = EDGE_CURVE ( 'NONE', #3674, #2748, #8459, .T. ) ;
#2907 = ORIENTED_EDGE ( 'NONE', *, *, #13701, .F. ) ;
#2908 = FACE_OUTER_BOUND ( 'NONE', #13294, .T. ) ;
#2909 = CYLINDRICAL_SURFACE ( 'NONE', #8330, 6.449999999999997513 ) ;
#2910 = EDGE_CURVE ( 'NONE', #7294, #10905, #4842, .T. ) ;
#2911 = DIRECTION ( 'NONE',  ( 0.000000000000000000, 0.000000000000000000, -1.000000000000000000 ) ) ;
#2912 = AXIS2_PLACEMENT_3D ( 'NONE', #10263, #7224, #4175 ) ;
#2913 = CARTESIAN_POINT ( 'NONE',  ( -1.059188295049996231, 27.97290950744599769, 17.25000000000000000 ) ) ;
#2914 = EDGE_CURVE ( 'NONE', #936, #8353, #11637, .T. ) ;
#2915 = ORIENTED_EDGE ( 'NONE', *, *, #2311, .T. ) ;
#2916 = ORIENTED_EDGE ( 'NONE', *, *, #1698, .F. ) ;
#2917 = CIRCLE ( 'NONE', #3575, 4.250000000000003553 ) ;
#2918 = AXIS2_PLACEMENT_3D ( 'NONE', #13033, #10114, #9048 ) ;
#2919 = VERTEX_POINT ( 'NONE', #10160 ) ;
#2920 = ORIENTED_EDGE ( 'NONE', *, *, #4571, .T. ) ;
#2921 = DIRECTION ( 'NONE',  ( -0.4528443260392609471, -0.8915896008669277339, 0.000000000000000000 ) ) ;
#2922 = ADVANCED_FACE ( 'NONE', ( #8821 ), #443, .T. ) ;
#2923 = CARTESIAN_POINT ( 'NONE',  ( -20.29752877034432146, 30.25218297742089035, 60.87931115570677321 ) ) ;
#2924 = DIRECTION ( 'NONE',  ( -1.000000000000000000, 0.000000000000000000, 0.000000000000000000 ) ) ;
#2925 = CARTESIAN_POINT ( 'NONE',  ( -22.64501676333060232, -4.028726038184999858, 63.45000000000000284 ) ) ;
#2926 = CARTESIAN_POINT ( 'NONE',  ( 134.6356359024541973, 103.9054980190242361, 23.00000000000000000 ) ) ;
#2927 = CARTESIAN_POINT ( 'NONE',  ( 16.04064420431708982, 4.500000000000000000, 9.307586582922137808 ) ) ;
#2928 = CARTESIAN_POINT ( 'NONE',  ( -18.05918829505001710, 10.97290950744599058, 98.85000000000000853 ) ) ;
#2929 = VERTEX_POINT ( 'NONE', #6932 ) ;
#2930 = EDGE_CURVE ( 'NONE', #1821, #12100, #13082, .T. ) ;
#2931 = AXIS2_PLACEMENT_3D ( 'NONE', #13507, #4029, #7010 ) ;
#2932 = ORIENTED_EDGE ( 'NONE', *, *, #10775, .F. ) ;
#2933 = DIRECTION ( 'NONE',  ( 0.6615960714621564875, -0.7498604124941129490, 0.000000000000000000 ) ) ;
#2934 = DIRECTION ( 'NONE',  ( 0.000000000000000000, 0.000000000000000000, 1.000000000000000000 ) ) ;
#2935 = VERTEX_POINT ( 'NONE', #1351 ) ;
#2936 = DIRECTION ( 'NONE',  ( 0.000000000000000000, 0.000000000000000000, -1.000000000000000000 ) ) ;
#2937 = CARTESIAN_POINT ( 'NONE',  ( -35.05918829505000645, 27.97290950744599769, 7.250000000000000000 ) ) ;
#2938 = DIRECTION ( 'NONE',  ( 0.000000000000000000, -1.000000000000000000, 0.000000000000000000 ) ) ;
#2939 = AXIS2_PLACEMENT_3D ( 'NONE', #9303, #7250, #9507 ) ;
#2940 = AXIS2_PLACEMENT_3D ( 'NONE', #10100, #12390, #715 ) ;
#2941 = LINE ( 'NONE', #4875, #10546 ) ;
#2942 = FACE_OUTER_BOUND ( 'NONE', #13551, .T. ) ;
#2943 = AXIS2_PLACEMENT_3D ( 'NONE', #4912, #2773, #1842 ) ;
#2944 = DIRECTION ( 'NONE',  ( 0.000000000000000000, 0.000000000000000000, -1.000000000000000000 ) ) ;
#2945 = DIRECTION ( 'NONE',  ( 0.7091883091770476710, -0.7050191076322684935, 0.000000000000000000 ) ) ;
#2946 = DIRECTION ( 'NONE',  ( 0.000000000000000000, 0.000000000000000000, -1.000000000000000000 ) ) ;
#2947 = DIRECTION ( 'NONE',  ( 1.000000000000000000, 0.000000000000000000, 0.000000000000000000 ) ) ;
#2948 = EDGE_CURVE ( 'NONE', #1179, #10331, #8244, .T. ) ;
#2949 = AXIS2_PLACEMENT_3D ( 'NONE', #1624, #8770, #3406 ) ;
#2950 = AXIS2_PLACEMENT_3D ( 'NONE', #9856, #9918, #2390 ) ;
#2951 = VECTOR ( 'NONE', #10113, 1000.000000000000000 ) ;
#2952 = VERTEX_POINT ( 'NONE', #5881 ) ;
#2953 = ORIENTED_EDGE ( 'NONE', *, *, #5984, .F. ) ;
#2954 = DIRECTION ( 'NONE',  ( 0.000000000000000000, 1.000000000000000000, 0.000000000000000000 ) ) ;
#2955 = EDGE_LOOP ( 'NONE', ( #11393, #1974, #8040, #8349 ) ) ;
#2956 = ORIENTED_EDGE ( 'NONE', *, *, #61, .F. ) ;
#2957 = ORIENTED_EDGE ( 'NONE', *, *, #3611, .T. ) ;
#2958 = DIRECTION ( 'NONE',  ( 1.000000000000000000, 0.000000000000000000, 0.000000000000000000 ) ) ;
#2959 = DIRECTION ( 'NONE',  ( 0.000000000000000000, -1.000000000000000000, 0.000000000000000000 ) ) ;
#2960 = CARTESIAN_POINT ( 'NONE',  ( -18.05918829504999934, 10.97290950744599947, 6.250000000000000000 ) ) ;
#2961 = DIRECTION ( 'NONE',  ( 1.000000000000000000, 0.000000000000000000, 0.000000000000000000 ) ) ;
#2962 = VECTOR ( 'NONE', #13332, 1000.000000000000000 ) ;
#2963 = FACE_OUTER_BOUND ( 'NONE', #9811, .T. ) ;
#2964 = CYLINDRICAL_SURFACE ( 'NONE', #1564, 1.999999999999991340 ) ;
#2965 = EDGE_CURVE ( 'NONE', #13584, #12422, #13356, .T. ) ;
#2966 = ADVANCED_FACE ( 'NONE', ( #5606, #9890 ), #4636, .T. ) ;
#2967 = EDGE_LOOP ( 'NONE', ( #12494, #12349 ) ) ;
#2968 = EDGE_CURVE ( 'NONE', #8660, #6154, #203, .T. ) ;
#2969 = AXIS2_PLACEMENT_3D ( 'NONE', #9702, #2173, #11667 ) ;
#2970 = CARTESIAN_POINT ( 'NONE',  ( -15.42197072176424122, 30.21012672847304614, 60.50206344250329238 ) ) ;
#2971 = EDGE_CURVE ( 'NONE', #6126, #10507, #4716, .T. ) ;
#2972 = VERTEX_POINT ( 'NONE', #713 ) ;
#2973 = LINE ( 'NONE', #6140, #5709 ) ;
#2974 = DIRECTION ( 'NONE',  ( -0.000000000000000000, -0.000000000000000000, -1.000000000000000000 ) ) ;
#2975 = CARTESIAN_POINT ( 'NONE',  ( -18.05918829504999934, 2.872909508741170015, 63.35000000000700027 ) ) ;
#2976 = ORIENTED_EDGE ( 'NONE', *, *, #5277, .F. ) ;
#2977 = ORIENTED_EDGE ( 'NONE', *, *, #8408, .F. ) ;
#2978 = DIRECTION ( 'NONE',  ( -1.000000000000000000, 0.000000000000000000, 0.000000000000000000 ) ) ;
#2979 = DIRECTION ( 'NONE',  ( 0.000000000000000000, 0.000000000000000000, -1.000000000000000000 ) ) ;
#2980 = ORIENTED_EDGE ( 'NONE', *, *, #6977, .T. ) ;
#2981 = LINE ( 'NONE', #8049, #8480 ) ;
#2982 = DIRECTION ( 'NONE',  ( 0.000000000000000000, 0.000000000000000000, 1.000000000000000000 ) ) ;
#2983 = CARTESIAN_POINT ( 'NONE',  ( 8.000000000000000000, -1.762812401309176307E-15, -65.00000000000000000 ) ) ;
#2984 = CARTESIAN_POINT ( 'NONE',  ( -16.08092853089235774, 4.500000000000000000, 9.237812082545083570 ) ) ;
#2985 = VECTOR ( 'NONE', #4317, 1000.000000000000000 ) ;
#2986 = ORIENTED_EDGE ( 'NONE', *, *, #9366, .F. ) ;
#2987 = EDGE_CURVE ( 'NONE', #4661, #12066, #11474, .T. ) ;
#2988 = ORIENTED_EDGE ( 'NONE', *, *, #2309, .F. ) ;
#2989 = VECTOR ( 'NONE', #11354, 1000.000000000000000 ) ;
#2990 = ORIENTED_EDGE ( 'NONE', *, *, #9369, .T. ) ;
#2991 = CARTESIAN_POINT ( 'NONE',  ( -25.86749127492454647, -8.860076549334127805, 83.57661607529820458 ) ) ;
#2992 = EDGE_CURVE ( 'NONE', #7369, #12154, #7549, .T. ) ;
#2993 = ORIENTED_EDGE ( 'NONE', *, *, #12512, .F. ) ;
#2994 = CARTESIAN_POINT ( 'NONE',  ( -18.59029969833234475, 30.35571874317119168, 61.67763804039374520 ) ) ;
#2995 = DIRECTION ( 'NONE',  ( -0.000000000000000000, -0.000000000000000000, 1.000000000000000000 ) ) ;
#2996 = DIRECTION ( 'NONE',  ( 1.000000000000000000, -0.000000000000000000, 0.000000000000000000 ) ) ;
#2997 = DIRECTION ( 'NONE',  ( 0.000000000000000000, 0.000000000000000000, 1.000000000000000000 ) ) ;
#2998 = FACE_BOUND ( 'NONE', #2276, .T. ) ;
#2999 = PRODUCT_CONTEXT ( 'NONE', #4316, 'mechanical' ) ;
#3000 = VERTEX_POINT ( 'NONE', #2839 ) ;
#3001 = EDGE_CURVE ( 'NONE', #349, #4986, #5116, .T. ) ;
#3002 = EDGE_CURVE ( 'NONE', #1587, #6209, #6229, .T. ) ;
#3003 = DIRECTION ( 'NONE',  ( 0.4528443260392608916, 0.8915896008669279560, 0.000000000000000000 ) ) ;
#3004 = CARTESIAN_POINT ( 'NONE',  ( -27.49999999999998934, 9.000000000000000000, -30.00000000000000355 ) ) ;
#3005 = VERTEX_POINT ( 'NONE', #8263 ) ;
#3006 = DIRECTION ( 'NONE',  ( -0.000000000000000000, -1.000000000000000000, -0.000000000000000000 ) ) ;
#3007 = DIRECTION ( 'NONE',  ( 0.000000000000000000, -0.000000000000000000, -1.000000000000000000 ) ) ;
#3008 = EDGE_CURVE ( 'NONE', #11514, #7434, #2917, .T. ) ;
#3009 = CIRCLE ( 'NONE', #7202, 16.95000000000000284 ) ;
#3010 = DIRECTION ( 'NONE',  ( 0.000000000000000000, 0.000000000000000000, -1.000000000000000000 ) ) ;
#3011 = CARTESIAN_POINT ( 'NONE',  ( 0.000000000000000000, 0.000000000000000000, 0.000000000000000000 ) ) ;
#3012 = DIRECTION ( 'NONE',  ( -1.000000000000000000, 0.000000000000000000, 0.000000000000000000 ) ) ;
#3013 = CARTESIAN_POINT ( 'NONE',  ( -18.05918829504999934, 10.97290950744599947, 61.72253826518770836 ) ) ;
#3014 = DIRECTION ( 'NONE',  ( 0.000000000000000000, 0.000000000000000000, -1.000000000000000000 ) ) ;
#3015 = CARTESIAN_POINT ( 'NONE',  ( 50.63563590245420443, 103.9054980190242361, 20.00000000000000000 ) ) ;
#3016 = DIRECTION ( 'NONE',  ( 0.000000000000000000, 0.000000000000000000, 1.000000000000000000 ) ) ;
#3017 = VERTEX_POINT ( 'NONE', #2983 ) ;
#3018 = EDGE_CURVE ( 'NONE', #12033, #11479, #11373, .T. ) ;
#3019 = EDGE_LOOP ( 'NONE', ( #11322, #146 ) ) ;
#3020 = ORIENTED_EDGE ( 'NONE', *, *, #7468, .T. ) ;
#3021 = ORIENTED_EDGE ( 'NONE', *, *, #9218, .T. ) ;
#3022 = DIRECTION ( 'NONE',  ( 1.000000000000000000, 0.000000000000000000, 0.000000000000000000 ) ) ;
#3023 = ORIENTED_EDGE ( 'NONE', *, *, #8616, .F. ) ;
#3024 = ORIENTED_EDGE ( 'NONE', *, *, #4670, .F. ) ;
#3025 = DIRECTION ( 'NONE',  ( 0.000000000000000000, 0.000000000000000000, -1.000000000000000000 ) ) ;
#3026 = EDGE_CURVE ( 'NONE', #10962, #1000, #1099, .T. ) ;
#3027 = COLOUR_RGB ( '', 0.09019608, 0.27058824, 0.51372549) ;
#3028 = LINE ( 'NONE', #2107, #8280 ) ;
#3029 = CARTESIAN_POINT ( 'NONE',  ( -39.80918829504999934, -6.027090492554000534, 64.85000000000000853 ) ) ;
#3030 = CYLINDRICAL_SURFACE ( 'NONE', #9554, 2.999999999999999112 ) ;
#3031 = CYLINDRICAL_SURFACE ( 'NONE', #5960, 0.4999999999999991673 ) ;
#3032 = ORIENTED_EDGE ( 'NONE', *, *, #9599, .T. ) ;
#3033 = CARTESIAN_POINT ( 'NONE',  ( -15.47476843086678677, 30.21612105669994364, 60.55881087961125075 ) ) ;
#3034 = ORIENTED_EDGE ( 'NONE', *, *, #8529, .T. ) ;
#3035 = DIRECTION ( 'NONE',  ( 0.9496839325805418452, -0.3132098788326394545, 0.000000000000000000 ) ) ;
#3036 = AXIS2_PLACEMENT_3D ( 'NONE', #4492, #8746, #11960 ) ;
#3037 = DIRECTION ( 'NONE',  ( 0.000000000000000000, 1.000000000000000000, 0.000000000000000000 ) ) ;
#3038 = VERTEX_POINT ( 'NONE', #5039 ) ;
#3039 = EDGE_LOOP ( 'NONE', ( #3401, #1357, #4355, #2035 ) ) ;
#3040 = CARTESIAN_POINT ( 'NONE',  ( 44.94629607423406270, 112.2890816101113387, 20.00000000000000000 ) ) ;
#3041 = DIRECTION ( 'NONE',  ( 0.000000000000000000, 0.000000000000000000, -1.000000000000000000 ) ) ;
#3042 = DIRECTION ( 'NONE',  ( 0.000000000000000000, 0.000000000000000000, -1.000000000000000000 ) ) ;
#3043 = CARTESIAN_POINT ( 'NONE',  ( -18.45035643575574014, 27.96940014844277300, 58.81168696388461825 ) ) ;
#3044 = EDGE_CURVE ( 'NONE', #5798, #1784, #1987, .T. ) ;
#3045 = FACE_OUTER_BOUND ( 'NONE', #6658, .T. ) ;
#3046 = VERTEX_POINT ( 'NONE', #6018 ) ;
#3047 = EDGE_LOOP ( 'NONE', ( #398, #4815, #9826, #2976 ) ) ;
#3048 = ORIENTED_EDGE ( 'NONE', *, *, #10549, .F. ) ;
#3049 = ORIENTED_EDGE ( 'NONE', *, *, #1038, .F. ) ;
#3050 = ORIENTED_EDGE ( 'NONE', *, *, #8509, .T. ) ;
#3051 = EDGE_LOOP ( 'NONE', ( #9574, #10179, #6442, #7215 ) ) ;
#3052 = ORIENTED_EDGE ( 'NONE', *, *, #12850, .T. ) ;
#3053 = LINE ( 'NONE', #2991, #160 ) ;
#3054 = VECTOR ( 'NONE', #10800, 1000.000000000000000 ) ;
#3055 = CARTESIAN_POINT ( 'NONE',  ( -19.00868903206585259, 30.34086823226316909, 61.57150343037032059 ) ) ;
#3056 = CARTESIAN_POINT ( 'NONE',  ( -18.94953701706641525, 26.94812814264477652, 56.14277197085647231 ) ) ;
#3057 = DIRECTION ( 'NONE',  ( 0.000000000000000000, 0.000000000000000000, 1.000000000000000000 ) ) ;
#3058 = CARTESIAN_POINT ( 'NONE',  ( -18.45469220996244886, -1.832421873814834123, -3.000000000000000000 ) ) ;
#3059 = EDGE_CURVE ( 'NONE', #12910, #4496, #9360, .T. ) ;
#3060 = CARTESIAN_POINT ( 'NONE',  ( -5.789834139046019956, -5.598733283342819611, 7.250000000000000000 ) ) ;
#3061 = APPLICATION_PROTOCOL_DEFINITION ( 'draft international standard', 'automotive_design', 1998, #1443 ) ;
#3062 = VERTEX_POINT ( 'NONE', #6085 ) ;
#3063 = EDGE_CURVE ( 'NONE', #12738, #12630, #10930, .T. ) ;
#3064 = PRODUCT_RELATED_PRODUCT_CATEGORY ( 'part', '', ( #9660 ) ) ;
#3065 = VECTOR ( 'NONE', #1492, 1000.000000000000000 ) ;
#3066 = CARTESIAN_POINT ( 'NONE',  ( 140.6356359024541973, 113.0390816101113387, 19.25000000000000000 ) ) ;
#3067 = ORIENTED_EDGE ( 'NONE', *, *, #2971, .T. ) ;
#3068 = EDGE_LOOP ( 'NONE', ( #12650, #3380, #7473, #3172 ) ) ;
#3069 = PLANE ( 'NONE',  #470 ) ;
#3070 = DIRECTION ( 'NONE',  ( 0.000000000000000000, 0.000000000000000000, 1.000000000000000000 ) ) ;
#3071 = CARTESIAN_POINT ( 'NONE',  ( 7.500000000000000000, -1.762812401309176307E-15, 0.000000000000000000 ) ) ;
#3072 = LINE ( 'NONE', #3140, #2310 ) ;
#3073 = CARTESIAN_POINT ( 'NONE',  ( 44.63563590245420443, 103.9054980190242361, 22.75000000000000000 ) ) ;
#3074 = DIRECTION ( 'NONE',  ( 0.4528443260392610026, 0.8915896008669278450, 0.000000000000000000 ) ) ;
#3075 = CARTESIAN_POINT ( 'NONE',  ( -27.49999999999998934, 0.000000000000000000, 29.99999999999999645 ) ) ;
#3076 = EDGE_CURVE ( 'NONE', #11380, #9897, #8936, .T. ) ;
#3077 = CIRCLE ( 'NONE', #10199, 2.000000000000001776 ) ;
#3078 = DIRECTION ( 'NONE',  ( 1.000000000000000000, 0.000000000000000000, 0.000000000000000000 ) ) ;
#3079 = CARTESIAN_POINT ( 'NONE',  ( 1.940811704950003991, -6.027090492554000534, 10.00000000000000000 ) ) ;
#3080 = EDGE_LOOP ( 'NONE', ( #8248, #300 ) ) ;
#3081 = ADVANCED_FACE ( 'NONE', ( #7132 ), #8125, .T. ) ;
#3082 = FACE_OUTER_BOUND ( 'NONE', #12101, .T. ) ;
#3083 = CARTESIAN_POINT ( 'NONE',  ( -20.76614708744390470, 15.25248827153688680, 68.78616702919012482 ) ) ;
#3084 = EDGE_LOOP ( 'NONE', ( #11686, #5598, #11497, #3914 ) ) ;
#3085 = CARTESIAN_POINT ( 'NONE',  ( -12.00000000000000000, -2.500000000000000444, -65.00000000000000000 ) ) ;
#3086 = CARTESIAN_POINT ( 'NONE',  ( -11.91335496205000055, 10.97290950744599947, 60.60999999999999943 ) ) ;
#3087 = DIRECTION ( 'NONE',  ( 1.000000000000000000, 0.000000000000000000, 0.000000000000000000 ) ) ;
#3088 = EDGE_CURVE ( 'NONE', #12241, #8398, #12389, .T. ) ;
#3089 = DIRECTION ( 'NONE',  ( -0.4528443260392609471, -0.8915896008669278450, 0.000000000000000000 ) ) ;
#3090 = AXIS2_PLACEMENT_3D ( 'NONE', #7410, #1006, #2212 ) ;
#3091 = PRESENTATION_LAYER_ASSIGNMENT (  '', '', ( #6415 ) ) ;
#3092 = EDGE_CURVE ( 'NONE', #12738, #4329, #3298, .T. ) ;
#3093 = ORIENTED_EDGE ( 'NONE', *, *, #8691, .T. ) ;
#3094 = CARTESIAN_POINT ( 'NONE',  ( -14.66438022474483382, 30.11090903182021705, 55.34105990772840045 ) ) ;
#3095 = AXIS2_PLACEMENT_3D ( 'NONE', #13480, #3988, #7380 ) ;
#3096 = ORIENTED_EDGE ( 'NONE', *, *, #2244, .T. ) ;
#3097 = ORIENTED_EDGE ( 'NONE', *, *, #2344, .T. ) ;
#3098 = DIRECTION ( 'NONE',  ( 0.000000000000000000, 0.000000000000000000, -1.000000000000000000 ) ) ;
#3099 = CIRCLE ( 'NONE', #8884, 0.4999999999999991673 ) ;
#3100 = DIRECTION ( 'NONE',  ( -0.000000000000000000, -0.000000000000000000, 1.000000000000000000 ) ) ;
#3101 = DIRECTION ( 'NONE',  ( -1.000000000000000000, 0.000000000000000000, 0.000000000000000000 ) ) ;
#3102 = ORIENTED_EDGE ( 'NONE', *, *, #8920, .F. ) ;
#3103 = CARTESIAN_POINT ( 'NONE',  ( 109.1537879975201406, 115.4601262030644762, 19.25000000000000000 ) ) ;
#3104 = CARTESIAN_POINT ( 'NONE',  ( 7.640422211807137209, 16.89844320975774750, 0.000000000000000000 ) ) ;
#3105 = DIRECTION ( 'NONE',  ( 0.000000000000000000, 0.000000000000000000, 1.000000000000000000 ) ) ;
#3106 = CARTESIAN_POINT ( 'NONE',  ( -18.05918829504999223, 2.660265422445993622, 63.26601075299999621 ) ) ;
#3107 = LINE ( 'NONE', #7330, #2724 ) ;
#3108 = CIRCLE ( 'NONE', #8665, 7.833333332999988130 ) ;
#3109 = AXIS2_PLACEMENT_3D ( 'NONE', #12864, #85, #6579 ) ;
#3110 = VECTOR ( 'NONE', #5701, 1000.000000000000000 ) ;
#3111 = CIRCLE ( 'NONE', #12235, 7.166108729582679970 ) ;
#3112 = VERTEX_POINT ( 'NONE', #7449 ) ;
#3113 = ORIENTED_EDGE ( 'NONE', *, *, #8680, .F. ) ;
#3114 = ORIENTED_EDGE ( 'NONE', *, *, #299, .T. ) ;
#3115 = ORIENTED_EDGE ( 'NONE', *, *, #10827, .T. ) ;
#3116 = ADVANCED_FACE ( 'NONE', ( #6305 ), #4485, .F. ) ;
#3117 = ORIENTED_EDGE ( 'NONE', *, *, #6995, .F. ) ;
#3118 = AXIS2_PLACEMENT_3D ( 'NONE', #7153, #6166, #2856 ) ;
#3119 = AXIS2_PLACEMENT_3D ( 'NONE', #10208, #7952, #4897 ) ;
#3120 = CIRCLE ( 'NONE', #13128, 24.92993838181874722 ) ;
#3121 = CARTESIAN_POINT ( 'NONE',  ( -18.05918829504999934, 10.97290950744599947, 31.09999999999999787 ) ) ;
#3122 = CARTESIAN_POINT ( 'NONE',  ( 42.63563590245419732, 87.03908161011136713, 19.25000000000000000 ) ) ;
#3123 = AXIS2_PLACEMENT_3D ( 'NONE', #7561, #5271, #3333 ) ;
#3124 = LINE ( 'NONE', #89, #5157 ) ;
#3125 = CARTESIAN_POINT ( 'NONE',  ( -18.19085538481590447, 26.97290194241137584, 55.85005112132051863 ) ) ;
#3126 = DIRECTION ( 'NONE',  ( 0.000000000000000000, 0.000000000000000000, -1.000000000000000000 ) ) ;
#3127 = CARTESIAN_POINT ( 'NONE',  ( 68.49370948373500312, 85.78908161011133870, 20.00000000000000000 ) ) ;
#3128 = VERTEX_POINT ( 'NONE', #5307 ) ;
#3129 = AXIS2_PLACEMENT_3D ( 'NONE', #12848, #9579, #5378 ) ;
#3130 = AXIS2_PLACEMENT_3D ( 'NONE', #2927, #7077, #3747 ) ;
#3131 = EDGE_CURVE ( 'NONE', #11544, #11152, #4409, .T. ) ;
#3132 = AXIS2_PLACEMENT_3D ( 'NONE', #3203, #6534, #10801 ) ;
#3133 = ADVANCED_FACE ( 'NONE', ( #212 ), #3184, .T. ) ;
#3134 = DIRECTION ( 'NONE',  ( -0.000000000000000000, -0.000000000000000000, -1.000000000000000000 ) ) ;
#3135 = CARTESIAN_POINT ( 'NONE',  ( 12.00000000000000000, 2.500000000000000000, -65.00000000000000000 ) ) ;
#3136 = ORIENTED_EDGE ( 'NONE', *, *, #6291, .F. ) ;
#3137 = LINE ( 'NONE', #6334, #1124 ) ;
#3138 = CARTESIAN_POINT ( 'NONE',  ( -38.38077571930826082, -0.4981161769137699147, 83.57661607529820458 ) ) ;
#3139 = CARTESIAN_POINT ( 'NONE',  ( -25.05563313235659706, -2.802149825948039741, 60.65000000000000568 ) ) ;
#3140 = CARTESIAN_POINT ( 'NONE',  ( 140.6356359024541973, 104.1554980190242361, 23.00000000000000000 ) ) ;
#3141 = VERTEX_POINT ( 'NONE', #12731 ) ;
#3142 = CARTESIAN_POINT ( 'NONE',  ( 4.000000000000001776, 2.000000000000000000, -65.00000000000000000 ) ) ;
#3143 = CARTESIAN_POINT ( 'NONE',  ( -35.05918829505000645, -6.027090492554000534, 58.85000000000000142 ) ) ;
#3144 = DIRECTION ( 'NONE',  ( 1.000000000000000000, 0.000000000000000000, 0.000000000000000000 ) ) ;
#3145 = ORIENTED_EDGE ( 'NONE', *, *, #5943, .F. ) ;
#3146 = EDGE_CURVE ( 'NONE', #1109, #11822, #7394, .T. ) ;
#3147 = ORIENTED_EDGE ( 'NONE', *, *, #9899, .T. ) ;
#3148 = VECTOR ( 'NONE', #13453, 1000.000000000000000 ) ;
#3149 = LINE ( 'NONE', #3419, #2150 ) ;
#3150 = ORIENTED_EDGE ( 'NONE', *, *, #10856, .F. ) ;
#3151 = CIRCLE ( 'NONE', #4920, 3.000000000000002665 ) ;
#3152 = CIRCLE ( 'NONE', #8267, 10.00000000000000178 ) ;
#3153 = CIRCLE ( 'NONE', #6480, 1.999999999999994893 ) ;
#3154 = ORIENTED_EDGE ( 'NONE', *, *, #1696, .F. ) ;
#3155 = ORIENTED_EDGE ( 'NONE', *, *, #13454, .F. ) ;
#3156 = ORIENTED_EDGE ( 'NONE', *, *, #6086, .T. ) ;
#3157 = DIRECTION ( 'NONE',  ( 0.4528443260392610026, 0.8915896008669278450, 0.000000000000000000 ) ) ;
#3158 = ORIENTED_EDGE ( 'NONE', *, *, #10760, .T. ) ;
#3159 = LINE ( 'NONE', #6128, #18 ) ;
#3160 = CARTESIAN_POINT ( 'NONE',  ( 76.11748380738829667, 115.4601262030644762, 20.00000000000000000 ) ) ;
#3161 = DIRECTION ( 'NONE',  ( 0.000000000000000000, 0.000000000000000000, 1.000000000000000000 ) ) ;
#3162 = ADVANCED_FACE ( 'NONE', ( #9794 ), #1118, .F. ) ;
#3163 = DIRECTION ( 'NONE',  ( -0.000000000000000000, -0.000000000000000000, 1.000000000000000000 ) ) ;
#3164 = AXIS2_PLACEMENT_3D ( 'NONE', #777, #5033, #9305 ) ;
#3165 = AXIS2_PLACEMENT_3D ( 'NONE', #13386, #4743, #11033 ) ;
#3166 = AXIS2_PLACEMENT_3D ( 'NONE', #12823, #2446, #1295 ) ;
#3167 = VERTEX_POINT ( 'NONE', #12 ) ;
#3168 = EDGE_CURVE ( 'NONE', #8341, #8660, #9140, .T. ) ;
#3169 = FACE_OUTER_BOUND ( 'NONE', #13474, .T. ) ;
#3170 = ORIENTED_EDGE ( 'NONE', *, *, #11254, .F. ) ;
#3171 = EDGE_LOOP ( 'NONE', ( #9666, #6901 ) ) ;
#3172 = ORIENTED_EDGE ( 'NONE', *, *, #4934, .F. ) ;
#3173 = ORIENTED_EDGE ( 'NONE', *, *, #8156, .T. ) ;
#3174 = DIRECTION ( 'NONE',  ( 0.000000000000000000, 0.000000000000000000, -1.000000000000000000 ) ) ;
#3175 = MECHANICAL_DESIGN_GEOMETRIC_PRESENTATION_REPRESENTATION (  '', ( #6501 ), #11190 ) ;
#3176 = SURFACE_STYLE_FILL_AREA ( #10414 ) ;
#3177 = CONICAL_SURFACE ( 'NONE', #12081, 6.419999999999999929, 0.2165503049760889864 ) ;
#3178 = CYLINDRICAL_SURFACE ( 'NONE', #12308, 24.92993838181874722 ) ;
#3179 = AXIS2_PLACEMENT_3D ( 'NONE', #238, #5458, #1139 ) ;
#3180 = ORIENTED_EDGE ( 'NONE', *, *, #9472, .T. ) ;
#3181 = DIRECTION ( 'NONE',  ( -1.000000000000000000, -1.182766006347823109E-16, 0.000000000000000000 ) ) ;
#3182 = DIRECTION ( 'NONE',  ( 0.000000000000000000, 0.000000000000000000, 1.000000000000000000 ) ) ;
#3183 = ADVANCED_FACE ( 'NONE', ( #4350 ), #4455, .T. ) ;
#3184 = PLANE ( 'NONE',  #2687 ) ;
#3185 = DIRECTION ( 'NONE',  ( 1.000000000000000000, 0.000000000000000000, 0.000000000000000000 ) ) ;
#3186 = CIRCLE ( 'NONE', #6286, 1.999999999999994893 ) ;
#3187 = EDGE_LOOP ( 'NONE', ( #1198, #10556 ) ) ;
#3188 = EDGE_LOOP ( 'NONE', ( #3720, #11391, #585, #6231 ) ) ;
#3189 = ORIENTED_EDGE ( 'NONE', *, *, #847, .T. ) ;
#3190 = ORIENTED_EDGE ( 'NONE', *, *, #9452, .F. ) ;
#3191 = LINE ( 'NONE', #2136, #3972 ) ;
#3192 = CARTESIAN_POINT ( 'NONE',  ( -18.05918829504999934, 10.97290950744599947, 61.85000000000000142 ) ) ;
#3193 = VERTEX_POINT ( 'NONE', #6366 ) ;
#3194 = ADVANCED_FACE ( 'NONE', ( #9656 ), #2192, .T. ) ;
#3195 = PLANE ( 'NONE',  #9184 ) ;
#3196 = ADVANCED_FACE ( 'NONE', ( #12920 ), #11887, .F. ) ;
#3197 = CYLINDRICAL_SURFACE ( 'NONE', #517, 1.999999999999993117 ) ;
#3198 = DIRECTION ( 'NONE',  ( 1.000000000000000000, -0.000000000000000000, 0.000000000000000000 ) ) ;
#3199 = DIRECTION ( 'NONE',  ( 0.000000000000000000, 0.000000000000000000, 1.000000000000000000 ) ) ;
#3200 = DIRECTION ( 'NONE',  ( 0.000000000000000000, 0.000000000000000000, 1.000000000000000000 ) ) ;
#3201 = AXIS2_PLACEMENT_3D ( 'NONE', #7271, #12806, #11697 ) ;
#3202 = ORIENTED_EDGE ( 'NONE', *, *, #3026, .F. ) ;
#3203 = CARTESIAN_POINT ( 'NONE',  ( -18.05918829504999934, 10.97290950744599947, 6.250000000000000000 ) ) ;
#3204 = DIRECTION ( 'NONE',  ( -0.2000659497483225358, 0.000000000000000000, 0.9797824328652262604 ) ) ;
#3205 = DIRECTION ( 'NONE',  ( 0.000000000000000000, 0.000000000000000000, 1.000000000000000000 ) ) ;
#3206 = CARTESIAN_POINT ( 'NONE',  ( -20.43440950813489465, 30.23850757514860987, 53.93886540776640715 ) ) ;
#3207 = PRESENTATION_STYLE_ASSIGNMENT (( #5270 ) ) ;
#3208 = PLANE ( 'NONE',  #4680 ) ;
#3209 = LINE ( 'NONE', #4583, #12902 ) ;
#3210 = DIRECTION ( 'NONE',  ( -0.7071067811865451302, 0.7071067811865500152, -0.000000000000000000 ) ) ;
#3211 = AXIS2_PLACEMENT_3D ( 'NONE', #3669, #2632, #8124 ) ;
#3212 = DIRECTION ( 'NONE',  ( -1.000000000000000000, 0.000000000000000000, 0.000000000000000000 ) ) ;
#3213 = EDGE_CURVE ( 'NONE', #2573, #6884, #6509, .T. ) ;
#3214 = ADVANCED_FACE ( 'NONE', ( #9720 ), #1027, .T. ) ;
#3215 = B_SPLINE_CURVE_WITH_KNOTS ( 'NONE', 3,
 ( #7559, #7636, #42, #10731, #12958, #1217, #4315, #11919, #1153, #2371, #11980, #6596, #5470, #2155, #4377, #4242, #1291, #9832, #254, #8772, #4519, #9614, #13027, #6336, #8490, #5410, #171, #9747, #6538, #10659, #12759, #11846, #3206, #3270, #9686, #7422, #11711, #7479, #6392, #8622, #5338, #11771, #12884, #2301, #13301, #12264, #13094, #8983, #456, #324, #7916, #3615, #4788, #9114, #5620, #8908, #6745, #3740, #7777, #12190, #10037, #10948, #383, #2575, #11018, #4580, #13239, #13369, #7850, #11218, #1366, #11142, #5677, #3678, #6804, #4725, #9043, #12126, #3813, #2641, #4854, #7990, #4654, #6873, #1570, #9900, #13167, #5821, #10107, #5890, #527, #2716, #8833, #10173, #6943, #592, #11078, #8066, #1495, #12052, #2441, #5750, #1641, #6670, #9957, #2506, #3541, #1433, #12467, #11283, #8343, #5949, #4024, #1705, #942, #2923, #1858, #11421, #2850, #11482, #9465, #8131, #3885, #10433, #1920, #6095, #12340, #12540, #10367, #9320, #5051, #866, #8196, #3055, #11550, #7270, #7070, #4095, #2994, #7146, #10243 ),
 .UNSPECIFIED., .F., .F.,
 ( 4, 2, 1, 1, 2, 2, 2, 2, 1, 1, 2, 2, 2, 2, 1, 1, 1, 2, 2, 2, 2, 2, 2, 2, 1, 1, 2, 2, 2, 2, 1, 1, 2, 2, 2, 2, 1, 2, 2, 2, 2, 2, 1, 1, 2, 2, 2, 2, 1, 1, 2, 2, 2, 2, 1, 1, 1, 1, 2, 2, 2, 2, 1, 1, 2, 2, 2, 2, 1, 1, 2, 2, 2, 2, 1, 1, 2, 2, 2, 2, 1, 2, 2, 4 ),
 ( 0.000000000000000000, 0.03124999999999248518, 0.04687499999998832878, 0.05468749999998662875, 0.05859374999998540057, 0.06249999999998417932, 0.09374999999997543632, 0.1093749999999707873, 0.1171874999999681366, 0.1210937499999661798, 0.1230468749999651668, 0.1249999999999641537, 0.1562499999999368283, 0.1718749999999231726, 0.1796874999999160116, 0.1835937499999121536, 0.1855468749999106548, 0.1865234374999094891, 0.1874999999999083233, 0.2031249999998842315, 0.2109374999998713529, 0.2187499999998585021, 0.2343749999998327449, 0.2421874999998198941, 0.2460937499998124556, 0.2480468749998095412, 0.2490234374998080702, 0.2499999999998066269, 0.2812499999997721267, 0.2968749999997541966, 0.3046874999997454814, 0.3085937499997403743, 0.3105468749997369882, 0.3124999999997335465, 0.3437499999996858069, 0.3593749999996613265, 0.3671874999996497246, 0.3710937499996447286, 0.3749999999996397881, 0.4999999999995009548, 0.5624999999994307887, 0.5937499999993955946, 0.6093749999993778310, 0.6171874999993681721, 0.6210937499993626210, 0.6249999999993569588, 0.6562499999993113287, 0.6718749999992886801, 0.6796874999992780220, 0.6835937499992728039, 0.6855468749992702504, 0.6874999999992676969, 0.7187499999992266186, 0.7343749999992060795, 0.7421874999991949773, 0.7460937499991895372, 0.7480468749991875388, 0.7490234374991859845, 0.7495117187491852073, 0.7499999999991844302, 0.7656249999992359445, 0.7734374999992611466, 0.7773437499992736921, 0.7792968749992797983, 0.7802734374992826849, 0.7812499999992855715, 0.7968749999993441913, 0.8046874999993740563, 0.8085937499993888222, 0.8105468749993962607, 0.8115234374994000355, 0.8124999999994038102, 0.8437499999995105027, 0.8593749999995646816, 0.8671874999995913269, 0.8710937499996049826, 0.8730468749996114219, 0.8749999999996178612, 0.9062499999997141176, 0.9218749999997626343, 0.9296874999997862821, 0.9335937499997979394, 0.9374999999998094857, 1.000000000000000000 ),
 .UNSPECIFIED. ) ;
#3216 = ORIENTED_EDGE ( 'NONE', *, *, #6210, .F. ) ;
#3217 = AXIS2_PLACEMENT_3D ( 'NONE', #13051, #2666, #3495 ) ;
#3218 = ORIENTED_EDGE ( 'NONE', *, *, #11649, .F. ) ;
#3219 = FACE_BOUND ( 'NONE', #1302, .T. ) ;
#3220 = ORIENTED_EDGE ( 'NONE', *, *, #10227, .T. ) ;
#3221 = ORIENTED_EDGE ( 'NONE', *, *, #4950, .T. ) ;
#3222 = ORIENTED_EDGE ( 'NONE', *, *, #2398, .F. ) ;
#3223 = CARTESIAN_POINT ( 'NONE',  ( -13.37752337641431133, 8.435598762370004167, 68.52507220045593783 ) ) ;
#3224 = FACE_OUTER_BOUND ( 'NONE', #4359, .T. ) ;
#3225 = EDGE_CURVE ( 'NONE', #4904, #6817, #1469, .T. ) ;
#3226 = CARTESIAN_POINT ( 'NONE',  ( 0.04028432657539327000, 4.500000000000000000, -18.54539866546729243 ) ) ;
#3227 = EDGE_CURVE ( 'NONE', #11675, #8158, #2254, .T. ) ;
#3228 = CARTESIAN_POINT ( 'NONE',  ( -26.45502162804999813, 10.97290950744599947, 60.75000000000000000 ) ) ;
#3229 = EDGE_CURVE ( 'NONE', #2636, #1997, #10001, .T. ) ;
#3230 = ADVANCED_FACE ( 'NONE', ( #1404 ), #7744, .F. ) ;
#3231 = UNCERTAINTY_MEASURE_WITH_UNIT (LENGTH_MEASURE( 1.000000000000000082E-05 ), #8984, 'distance_accuracy_value', 'NONE');
#3232 = ORIENTED_EDGE ( 'NONE', *, *, #7998, .F. ) ;
#3233 = CARTESIAN_POINT ( 'NONE',  ( -15.72734351507429018, 30.24295657546931437, 53.90012880255799388 ) ) ;
#3234 = ORIENTED_EDGE ( 'NONE', *, *, #7822, .T. ) ;
#3235 = EDGE_LOOP ( 'NONE', ( #6189, #6441, #9842, #9712, #11213, #11229 ) ) ;
#3236 = DIRECTION ( 'NONE',  ( 0.000000000000000000, 0.000000000000000000, 1.000000000000000000 ) ) ;
#3237 = CARTESIAN_POINT ( 'NONE',  ( 134.6356359024541973, 94.90549801902425031, 23.00000000000000000 ) ) ;
#3238 = DIRECTION ( 'NONE',  ( -0.000000000000000000, -0.000000000000000000, 1.000000000000000000 ) ) ;
#3239 = ORIENTED_EDGE ( 'NONE', *, *, #7622, .T. ) ;
#3240 = DIRECTION ( 'NONE',  ( 0.000000000000000000, 0.000000000000000000, -1.000000000000000000 ) ) ;
#3241 = LINE ( 'NONE', #13695, #10463 ) ;
#3242 = DIRECTION ( 'NONE',  ( 0.000000000000000000, 0.000000000000000000, 1.000000000000000000 ) ) ;
#3243 = EDGE_CURVE ( 'NONE', #12583, #6548, #5565, .T. ) ;
#3244 = CARTESIAN_POINT ( 'NONE',  ( -18.05918829504999934, 7.130333642789880244, 7.250000000000000000 ) ) ;
#3245 = ORIENTED_EDGE ( 'NONE', *, *, #12256, .T. ) ;
#3246 = ORIENTED_EDGE ( 'NONE', *, *, #10760, .F. ) ;
#3247 = ADVANCED_FACE ( 'NONE', ( #2411 ), #7954, .T. ) ;
#3248 = AXIS2_PLACEMENT_3D ( 'NONE', #6575, #5518, #17 ) ;
#3249 = CARTESIAN_POINT ( 'NONE',  ( -4.640588396653431147, -14.07073191448199978, 7.250000000000000000 ) ) ;
#3250 = ORIENTED_EDGE ( 'NONE', *, *, #13229, .T. ) ;
#3251 = ORIENTED_EDGE ( 'NONE', *, *, #7468, .F. ) ;
#3252 = VERTEX_POINT ( 'NONE', #502 ) ;
#3253 = DIRECTION ( 'NONE',  ( 0.000000000000000000, 0.000000000000000000, -1.000000000000000000 ) ) ;
#3254 = CARTESIAN_POINT ( 'NONE',  ( -25.86749127492454647, -8.860076549334124252, 17.25000000000000000 ) ) ;
#3255 = CARTESIAN_POINT ( 'NONE',  ( 44.63563590245419732, 94.90549801902423610, 22.89644660940672694 ) ) ;
#3256 = DIRECTION ( 'NONE',  ( 0.000000000000000000, 0.000000000000000000, -1.000000000000000000 ) ) ;
#3257 = DIRECTION ( 'NONE',  ( -1.000000000000000000, -1.792228749776982873E-15, 0.000000000000000000 ) ) ;
#3258 = DIRECTION ( 'NONE',  ( -1.000000000000000000, 0.000000000000000000, 0.000000000000000000 ) ) ;
#3259 = ADVANCED_FACE ( 'NONE', ( #6715 ), #427, .T. ) ;
#3260 = CARTESIAN_POINT ( 'NONE',  ( 142.6356359024541973, 87.03908161011133870, 19.25000000000000000 ) ) ;
#3262 = ADVANCED_FACE ( 'NONE', ( #8955 ), #5587, .T. ) ;
#3261 = ITEM_DEFINED_TRANSFORMATION ( 'NONE', 'NONE', #7535,  #6434 ) ;
#3263 = ADVANCED_FACE ( 'NONE', ( #6840 ), #9932, .T. ) ;
#3264 = EDGE_LOOP ( 'NONE', ( #9306, #10844, #10140, #12147 ) ) ;
#3265 = DIRECTION ( 'NONE',  ( 1.000000000000000000, 0.000000000000000000, 0.000000000000000000 ) ) ;
#3266 = VERTEX_POINT ( 'NONE', #4620 ) ;
#3267 = DIRECTION ( 'NONE',  ( -1.000000000000000000, 0.000000000000000000, 0.000000000000000000 ) ) ;
#3268 = DIRECTION ( 'NONE',  ( 0.000000000000000000, 1.000000000000000000, 0.000000000000000000 ) ) ;
#3269 = LINE ( 'NONE', #8832, #11329 ) ;
#3270 = CARTESIAN_POINT ( 'NONE',  ( -20.46141587662859607, 30.23571878071122399, 53.96345633405123721 ) ) ;
#3271 =( LENGTH_UNIT ( ) NAMED_UNIT ( * ) SI_UNIT ( .MILLI., .METRE. ) );
#3272 = ORIENTED_EDGE ( 'NONE', *, *, #9094, .F. ) ;
#3273 = CARTESIAN_POINT ( 'NONE',  ( -5.631644894983189431, 10.97290950744599947, 5.250000000000000000 ) ) ;
#3274 = DIRECTION ( 'NONE',  ( 0.000000000000000000, 0.000000000000000000, 1.000000000000000000 ) ) ;
#3275 = CARTESIAN_POINT ( 'NONE',  ( 140.5069562460138286, 85.34974178189114014, 20.00000000000000000 ) ) ;
#3276 = CARTESIAN_POINT ( 'NONE',  ( -12.00000000000000000, 2.500000000000000000, 0.000000000000000000 ) ) ;
#3277 = AXIS2_PLACEMENT_3D ( 'NONE', #8415, #11641, #1015 ) ;
#3278 = CYLINDRICAL_SURFACE ( 'NONE', #7241, 0.7500000000000006661 ) ;
#3279 = EDGE_CURVE ( 'NONE', #3533, #5517, #7889, .T. ) ;
#3280 = ORIENTED_EDGE ( 'NONE', *, *, #1286, .F. ) ;
#3281 = ORIENTED_EDGE ( 'NONE', *, *, #3801, .F. ) ;
#3282 = DIRECTION ( 'NONE',  ( 0.000000000000000000, 0.000000000000000000, 1.000000000000000000 ) ) ;
#3283 = AXIS2_PLACEMENT_3D ( 'NONE', #762, #2042, #3157 ) ;
#3284 = DIRECTION ( 'NONE',  ( -1.000000000000000000, 0.000000000000000000, 0.000000000000000000 ) ) ;
#3285 = CARTESIAN_POINT ( 'NONE',  ( -16.08092853089235774, 4.500000000000000000, 9.237812082545083570 ) ) ;
#3286 = CARTESIAN_POINT ( 'NONE',  ( -16.81378748857474292, 5.403809379663265133, 68.16287202337919382 ) ) ;
#3287 = DIRECTION ( 'NONE',  ( -0.000000000000000000, -0.000000000000000000, 1.000000000000000000 ) ) ;
#3288 = DIRECTION ( 'NONE',  ( 0.000000000000000000, 0.000000000000000000, -1.000000000000000000 ) ) ;
#3289 = DIRECTION ( 'NONE',  ( 0.000000000000000000, 0.000000000000000000, 1.000000000000000000 ) ) ;
#3290 = ADVANCED_FACE ( 'NONE', ( #1542 ), #12997, .T. ) ;
#3291 = ORIENTED_EDGE ( 'NONE', *, *, #7389, .T. ) ;
#3292 = DIRECTION ( 'NONE',  ( 0.000000000000000000, 0.000000000000000000, -1.000000000000000000 ) ) ;
#3293 = DIRECTION ( 'NONE',  ( 0.6615960714621565986, -0.7498604124941127269, 0.000000000000000000 ) ) ;
#3294 = CYLINDRICAL_SURFACE ( 'NONE', #682, 0.2500000000000002220 ) ;
#3295 = DIRECTION ( 'NONE',  ( -0.000000000000000000, -0.000000000000000000, -1.000000000000000000 ) ) ;
#3296 = DIRECTION ( 'NONE',  ( 1.000000000000000000, 0.000000000000000000, 0.000000000000000000 ) ) ;
#3297 = VECTOR ( 'NONE', #11433, 1000.000000000000000 ) ;
#3298 = LINE ( 'NONE', #7602, #3338 ) ;
#3299 = CARTESIAN_POINT ( 'NONE',  ( -1.059188295049996231, 27.97290950744599769, 58.85000000000000142 ) ) ;
#3300 = PRODUCT ( 'BR-Y-110', 'BR-Y-110', '', ( #2999 ) ) ;
#3301 = AXIS2_PLACEMENT_3D ( 'NONE', #12280, #1061, #12411 ) ;
#3302 = AXIS2_PLACEMENT_3D ( 'NONE', #253, #2640, #4517 ) ;
#3303 = FACE_OUTER_BOUND ( 'NONE', #1929, .T. ) ;
#3304 = ORIENTED_EDGE ( 'NONE', *, *, #3666, .T. ) ;
#3305 = ADVANCED_FACE ( 'NONE', ( #5862 ), #6778, .F. ) ;
#3306 = ORIENTED_EDGE ( 'NONE', *, *, #6909, .T. ) ;
#3307 = ORIENTED_EDGE ( 'NONE', *, *, #50, .T. ) ;
#3308 = CARTESIAN_POINT ( 'NONE',  ( 68.49370948373500312, 113.0390816101113387, 19.25000000000000000 ) ) ;
#3309 = DIRECTION ( 'NONE',  ( 0.000000000000000000, 0.000000000000000000, -1.000000000000000000 ) ) ;
#3310 = ORIENTED_EDGE ( 'NONE', *, *, #10363, .T. ) ;
#3311 = FACE_OUTER_BOUND ( 'NONE', #2766, .T. ) ;
#3312 = VECTOR ( 'NONE', #5291, 1000.000000000000114 ) ;
#3313 = DIRECTION ( 'NONE',  ( -0.000000000000000000, -0.000000000000000000, -1.000000000000000000 ) ) ;
#3314 = AXIS2_PLACEMENT_3D ( 'NONE', #5179, #3181, #4140 ) ;
#3315 = CYLINDRICAL_SURFACE ( 'NONE', #11993, 3.000000000000000000 ) ;
#3316 = CIRCLE ( 'NONE', #11348, 16.95000000000000284 ) ;
#3317 = DIRECTION ( 'NONE',  ( -0.000000000000000000, -0.000000000000000000, -1.000000000000000000 ) ) ;
#3318 = VECTOR ( 'NONE', #7407, 1000.000000000000000 ) ;
#3319 = EDGE_CURVE ( 'NONE', #12272, #5077, #3444, .T. ) ;
#3320 = FACE_OUTER_BOUND ( 'NONE', #2402, .T. ) ;
#3321 = APPLICATION_PROTOCOL_DEFINITION ( 'draft international standard', 'automotive_design', 1998, #12857 ) ;
#3322 = CONICAL_SURFACE ( 'NONE', #13339, 2.500000000000000000, 0.7853981633974532750 ) ;
#3323 = ORIENTED_EDGE ( 'NONE', *, *, #6326, .F. ) ;
#3324 = CIRCLE ( 'NONE', #10252, 6.000000000000000888 ) ;
#3325 = AXIS2_PLACEMENT_3D ( 'NONE', #459, #12130, #12055 ) ;
#3326 = ORIENTED_EDGE ( 'NONE', *, *, #11763, .F. ) ;
#3327 = ADVANCED_FACE ( 'NONE', ( #10992 ), #359, .F. ) ;
#3328 = DIRECTION ( 'NONE',  ( 1.000000000000000000, 0.000000000000000000, 0.000000000000000000 ) ) ;
#3329 = CARTESIAN_POINT ( 'NONE',  ( -5.789834139046009298, 27.54455229823479812, 68.85549045786049760 ) ) ;
#3330 = DIRECTION ( 'NONE',  ( 1.000000000000000000, 0.000000000000000000, 0.000000000000000000 ) ) ;
#3331 = DIRECTION ( 'NONE',  ( -1.000000000000000000, 0.000000000000000000, 0.000000000000000000 ) ) ;
#3332 = CARTESIAN_POINT ( 'NONE',  ( 44.63563590245421864, 85.03908161011133870, 0.7500000000000006661 ) ) ;
#3333 = DIRECTION ( 'NONE',  ( -1.000000000000000000, 0.000000000000000000, 0.000000000000000000 ) ) ;
#3334 = DIRECTION ( 'NONE',  ( 1.000000000000000000, 0.000000000000000000, 0.000000000000000000 ) ) ;
#3335 = ADVANCED_FACE ( 'NONE', ( #2889 ), #9230, .F. ) ;
#3336 = DIRECTION ( 'NONE',  ( 0.000000000000000000, -1.000000000000000000, 0.000000000000000000 ) ) ;
#3337 = AXIS2_PLACEMENT_3D ( 'NONE', #872, #660, #3823 ) ;
#3338 = VECTOR ( 'NONE', #1049, 1000.000000000000000 ) ;
#3339 = VECTOR ( 'NONE', #12815, 1000.000000000000000 ) ;
#3340 = ORIENTED_EDGE ( 'NONE', *, *, #5418, .F. ) ;
#3341 = ORIENTED_EDGE ( 'NONE', *, *, #5516, .F. ) ;
#3342 = CARTESIAN_POINT ( 'NONE',  ( 92.63563590245421153, 85.78908161011133870, 19.25000000000000000 ) ) ;
#3343 = EDGE_LOOP ( 'NONE', ( #5355, #571, #8847, #13069, #9284, #8231, #13676, #5582, #12581, #8099, #2168, #9530, #11277, #5885, #6832, #13165, #1162, #8173, #631, #10642 ) ) ;
#3344 = ORIENTED_EDGE ( 'NONE', *, *, #8167, .F. ) ;
#3345 = EDGE_LOOP ( 'NONE', ( #11250, #12664 ) ) ;
#3346 = ORIENTED_EDGE ( 'NONE', *, *, #9820, .F. ) ;
#3347 = PLANE ( 'NONE',  #1722 ) ;
#3348 = CARTESIAN_POINT ( 'NONE',  ( 92.63563590245421153, 99.03908161011133870, -30.00000000000001776 ) ) ;
#3349 = VECTOR ( 'NONE', #1444, 1000.000000000000000 ) ;
#3350 = VECTOR ( 'NONE', #13795, 1000.000000000000000 ) ;
#3351 = SURFACE_STYLE_USAGE ( .BOTH. , #58 ) ;
#3352 = DIRECTION ( 'NONE',  ( -1.000000000000000000, 0.000000000000000000, 0.000000000000000000 ) ) ;
#3353 = CARTESIAN_POINT ( 'NONE',  ( -5.309188295050000228, 27.97290950744599769, 64.35000000000000853 ) ) ;
#3354 = ADVANCED_FACE ( 'NONE', ( #5997 ), #3858, .F. ) ;
#3355 = CARTESIAN_POINT ( 'NONE',  ( -35.05918829505000645, 27.97290950744599769, 64.35000000000000853 ) ) ;
#3356 = DIRECTION ( 'NONE',  ( 0.000000000000000000, 0.000000000000000000, -1.000000000000000000 ) ) ;
#3357 = B_SPLINE_CURVE_WITH_KNOTS ( 'NONE', 3,
 ( #4616, #5857, #2678, #7883 ),
 .UNSPECIFIED., .F., .F.,
 ( 4, 4 ),
 ( 0.000000000000000000, 1.000000000000000000 ),
 .UNSPECIFIED. ) ;
#3358 = CIRCLE ( 'NONE', #12045, 2.000000000000001776 ) ;
#3359 = AXIS2_PLACEMENT_3D ( 'NONE', #8802, #13131, #4347 ) ;
#3360 = AXIS2_PLACEMENT_3D ( 'NONE', #9891, #649, #4783 ) ;
#3361 = ORIENTED_EDGE ( 'NONE', *, *, #12048, .F. ) ;
#3362 = CARTESIAN_POINT ( 'NONE',  ( -15.26746632920534807, 30.19191053447994832, 54.37610708475375532 ) ) ;
#3363 = ORIENTED_EDGE ( 'NONE', *, *, #8433, .F. ) ;
#3364 = EDGE_LOOP ( 'NONE', ( #10236, #12436 ) ) ;
#3365 = CARTESIAN_POINT ( 'NONE',  ( -25.86749127492454647, -8.860076549334127805, 5.250000000000000000 ) ) ;
#3366 = CARTESIAN_POINT ( 'NONE',  ( -1.059188295049996231, -6.027090492554000534, 0.000000000000000000 ) ) ;
#3367 = DIRECTION ( 'NONE',  ( -1.000000000000000000, 0.000000000000000000, 0.000000000000000000 ) ) ;
#3368 = ORIENTED_EDGE ( 'NONE', *, *, #2712, .T. ) ;
#3369 = CARTESIAN_POINT ( 'NONE',  ( 42.63563590245419732, 85.03908161011133870, 0.7500000000000006661 ) ) ;
#3370 = DIRECTION ( 'NONE',  ( -1.000000000000000000, -0.000000000000000000, 0.000000000000000000 ) ) ;
#3371 = CIRCLE ( 'NONE', #5132, 15.45000000000000462 ) ;
#3372 = AXIS2_PLACEMENT_3D ( 'NONE', #11592, #10401, #2043 ) ;
#3373 = VECTOR ( 'NONE', #2193, 1000.000000000000000 ) ;
#3374 = CIRCLE ( 'NONE', #10066, 0.5000000000000004441 ) ;
#3375 = CARTESIAN_POINT ( 'NONE',  ( -5.631644894983189431, 10.97290950744599947, 83.57661607529820458 ) ) ;
#3376 = ADVANCED_FACE ( 'NONE', ( #9295 ), #2964, .F. ) ;
#3377 = EDGE_CURVE ( 'NONE', #9938, #10214, #4465, .T. ) ;
#3378 = ORIENTED_EDGE ( 'NONE', *, *, #5201, .F. ) ;
#3379 = AXIS2_PLACEMENT_3D ( 'NONE', #6076, #3931, #3101 ) ;
#3380 = ORIENTED_EDGE ( 'NONE', *, *, #2226, .T. ) ;
#3381 = DIRECTION ( 'NONE',  ( -0.7071067811865520136, 0.7071067811865429098, 0.000000000000000000 ) ) ;
#3382 = AXIS2_PLACEMENT_3D ( 'NONE', #8294, #12689, #5545 ) ;
#3383 = CIRCLE ( 'NONE', #5158, 4.749999999999997335 ) ;
#3384 = ORIENTED_EDGE ( 'NONE', *, *, #8868, .T. ) ;
#3385 = ORIENTED_EDGE ( 'NONE', *, *, #12200, .F. ) ;
#3386 = ORIENTED_EDGE ( 'NONE', *, *, #3279, .T. ) ;
#3387 = CARTESIAN_POINT ( 'NONE',  ( -32.35918829505000360, -6.027090492554000534, 64.85000000000000853 ) ) ;
#3388 = FACE_OUTER_BOUND ( 'NONE', #10319, .T. ) ;
#3389 = VERTEX_POINT ( 'NONE', #6069 ) ;
#3390 = DIRECTION ( 'NONE',  ( 0.000000000000000000, -1.000000000000000000, 2.732534507816519619E-15 ) ) ;
#3391 = CARTESIAN_POINT ( 'NONE',  ( -5.631644894983189431, 10.97290950744599947, 17.25000000000000000 ) ) ;
#3392 = DIRECTION ( 'NONE',  ( 0.000000000000000000, 0.000000000000000000, 1.000000000000000000 ) ) ;
#3393 = DIRECTION ( 'NONE',  ( -0.000000000000000000, 1.000000000000000000, -0.000000000000000000 ) ) ;
#3394 = PLANE ( 'NONE',  #7794 ) ;
#3395 = CONICAL_SURFACE ( 'NONE', #1141, 16.00000000000000000, 0.7853981633974476129 ) ;
#3396 = AXIS2_PLACEMENT_3D ( 'NONE', #11205, #11968, #1421 ) ;
#3397 = EDGE_LOOP ( 'NONE', ( #10408, #8059, #549, #7608 ) ) ;
#3398 = AXIS2_PLACEMENT_3D ( 'NONE', #4732, #8987, #658 ) ;
#3399 = ADVANCED_FACE ( 'NONE', ( #9158 ), #10343, .T. ) ;
#3400 = ORIENTED_EDGE ( 'NONE', *, *, #12092, .T. ) ;
#3401 = ORIENTED_EDGE ( 'NONE', *, *, #7558, .T. ) ;
#3402 = COLOUR_RGB ( '', 0.09019608, 0.27058824, 0.51372549) ;
#3403 = CARTESIAN_POINT ( 'NONE',  ( -5.631644894983189431, 10.97290950744599947, 17.25000000000000000 ) ) ;
#3404 = CARTESIAN_POINT ( 'NONE',  ( 134.8856359024541973, 90.15549801902423610, 23.00000000000000000 ) ) ;
#3405 = ORIENTED_EDGE ( 'NONE', *, *, #4813, .F. ) ;
#3406 = DIRECTION ( 'NONE',  ( 1.000000000000000000, 0.000000000000000000, 0.000000000000000000 ) ) ;
#3407 = DIRECTION ( 'NONE',  ( 0.000000000000000000, 0.000000000000000000, 1.000000000000000000 ) ) ;
#3408 = CARTESIAN_POINT ( 'NONE',  ( -28.87730642030694739, 29.81324547859995278, 83.57661607529820458 ) ) ;
#3409 = ORIENTED_EDGE ( 'NONE', *, *, #5244, .F. ) ;
#3410 = CARTESIAN_POINT ( 'NONE',  ( -18.05918829504999934, 10.97290950744599947, 61.10999999999999943 ) ) ;
#3411 = LINE ( 'NONE', #11577, #1076 ) ;
#3412 = CARTESIAN_POINT ( 'NONE',  ( 12.00000000000000000, -2.499999999999999556, -65.00000000000000000 ) ) ;
#3413 = FACE_BOUND ( 'NONE', #10987, .T. ) ;
#3414 = ADVANCED_FACE ( 'NONE', ( #769 ), #9364, .T. ) ;
#3415 = AXIS2_PLACEMENT_3D ( 'NONE', #6746, #13168, #9749 ) ;
#3416 = ADVANCED_FACE ( 'NONE', ( #3921 ), #8108, .F. ) ;
#3417 = ORIENTED_EDGE ( 'NONE', *, *, #904, .F. ) ;
#3418 = EDGE_CURVE ( 'NONE', #12860, #135, #7181, .T. ) ;
#3419 = CARTESIAN_POINT ( 'NONE',  ( -28.87730642030694739, 29.81324547859995278, 5.250000000000000000 ) ) ;
#3420 = VERTEX_POINT ( 'NONE', #6134 ) ;
#3421 = ORIENTED_EDGE ( 'NONE', *, *, #6752, .T. ) ;
#3422 = LINE ( 'NONE', #11030, #8266 ) ;
#3423 = DIRECTION ( 'NONE',  ( 0.000000000000000000, 0.000000000000000000, 1.000000000000000000 ) ) ;
#3424 = DIRECTION ( 'NONE',  ( 0.000000000000000000, -0.000000000000000000, 1.000000000000000000 ) ) ;
#3425 = AXIS2_PLACEMENT_3D ( 'NONE', #4992, #593, #1787 ) ;
#3426 = DIRECTION ( 'NONE',  ( 0.000000000000000000, 0.000000000000000000, -1.000000000000000000 ) ) ;
#3427 = DIRECTION ( 'NONE',  ( -0.3132098788326400096, -0.9496839325805418452, 0.000000000000000000 ) ) ;
#3428 = VERTEX_POINT ( 'NONE', #830 ) ;
#3429 = CARTESIAN_POINT ( 'NONE',  ( 142.6356359024541973, 111.0390816101113245, 19.25000000000000000 ) ) ;
#3430 = CARTESIAN_POINT ( 'NONE',  ( 92.63563590245421153, 99.03908161011133870, 0.7500000000000006661 ) ) ;
#3431 = DIRECTION ( 'NONE',  ( -1.000000000000000000, 0.000000000000000000, 0.000000000000000000 ) ) ;
#3432 = CARTESIAN_POINT ( 'NONE',  ( -18.05918829504999934, 10.97290950744599947, 64.54999999999999716 ) ) ;
#3433 = EDGE_CURVE ( 'NONE', #6919, #10012, #9381, .T. ) ;
#3434 = AXIS2_PLACEMENT_3D ( 'NONE', #12906, #10421, #3042 ) ;
#3435 = EDGE_LOOP ( 'NONE', ( #3848, #2692, #933, #1817 ) ) ;
#3436 = ADVANCED_FACE ( 'NONE', ( #3783 ), #5347, .F. ) ;
#3437 = CARTESIAN_POINT ( 'NONE',  ( -16.76578548723817974, 30.32455137611084339, 53.24728338428077734 ) ) ;
#3438 = ORIENTED_EDGE ( 'NONE', *, *, #12712, .F. ) ;
#3439 = DIRECTION ( 'NONE',  ( -1.000000000000000000, 0.000000000000000000, 0.000000000000000000 ) ) ;
#3440 = DIRECTION ( 'NONE',  ( 0.000000000000000000, 0.000000000000000000, 1.000000000000000000 ) ) ;
#3441 = DIRECTION ( 'NONE',  ( 1.000000000000000000, 0.000000000000000000, 0.000000000000000000 ) ) ;
#3442 = PLANE ( 'NONE',  #4890 ) ;
#3443 = CIRCLE ( 'NONE', #12792, 2.000000000000001776 ) ;
#3444 = LINE ( 'NONE', #293, #2479 ) ;
#3445 = CARTESIAN_POINT ( 'NONE',  ( 74.18094369249178044, 97.20665973629650125, 10.00000000000000000 ) ) ;
#3446 = VERTEX_POINT ( 'NONE', #4899 ) ;
#3447 = ORIENTED_EDGE ( 'NONE', *, *, #1060, .T. ) ;
#3448 = EDGE_LOOP ( 'NONE', ( #9481, #9079 ) ) ;
#3449 = PLANE ( 'NONE',  #7908 ) ;
#3450 = ORIENTED_EDGE ( 'NONE', *, *, #6475, .F. ) ;
#3451 = VERTEX_POINT ( 'NONE', #1750 ) ;
#3452 = EDGE_LOOP ( 'NONE', ( #1417, #2203, #3447, #799 ) ) ;
#3453 = ORIENTED_EDGE ( 'NONE', *, *, #1091, .F. ) ;
#3454 = PLANE ( 'NONE',  #10436 ) ;
#3455 = EDGE_CURVE ( 'NONE', #11963, #3647, #4031, .T. ) ;
#3456 = DIRECTION ( 'NONE',  ( 0.000000000000000000, 1.000000000000000000, -0.000000000000000000 ) ) ;
#3457 = ORIENTED_EDGE ( 'NONE', *, *, #13134, .T. ) ;
#3458 = CARTESIAN_POINT ( 'NONE',  ( 5.640422211807141650, 16.89844320975774750, 7.000000000000000000 ) ) ;
#3459 = CARTESIAN_POINT ( 'NONE',  ( 134.6356359024541973, 89.90549801902423610, 23.00000000000000000 ) ) ;
#3460 = DIRECTION ( 'NONE',  ( 1.000000000000000000, 0.000000000000000000, 0.000000000000000000 ) ) ;
#3461 = CARTESIAN_POINT ( 'NONE',  ( -18.05918829504999934, 10.97290950744599947, 62.14999999999999858 ) ) ;
#3462 = DIRECTION ( 'NONE',  ( -0.000000000000000000, -0.000000000000000000, 1.000000000000000000 ) ) ;
#3463 = ORIENTED_EDGE ( 'NONE', *, *, #9366, .T. ) ;
#3464 = ORIENTED_EDGE ( 'NONE', *, *, #12753, .F. ) ;
#3465 = CARTESIAN_POINT ( 'NONE',  ( -11.74835982676941981, -4.028726038184999858, 63.45000000000000284 ) ) ;
#3466 = DIRECTION ( 'NONE',  ( -0.000000000000000000, -1.000000000000000000, -0.000000000000000000 ) ) ;
#3467 = ORIENTED_EDGE ( 'NONE', *, *, #865, .F. ) ;
#3468 = DIRECTION ( 'NONE',  ( -1.000000000000000000, 0.000000000000000000, 0.000000000000000000 ) ) ;
#3469 = EDGE_CURVE ( 'NONE', #722, #3590, #4964, .T. ) ;
#3470 =( NAMED_UNIT ( * ) SI_UNIT ( $, .STERADIAN. ) SOLID_ANGLE_UNIT ( ) );
#3471 = CIRCLE ( 'NONE', #8577, 2.700000000000000178 ) ;
#3472 = PLANE ( 'NONE',  #5823 ) ;
#3473 = FACE_OUTER_BOUND ( 'NONE', #5597, .T. ) ;
#3474 = DIRECTION ( 'NONE',  ( 0.000000000000000000, 1.000000000000000000, 0.000000000000000000 ) ) ;
#3475 = CARTESIAN_POINT ( 'NONE',  ( -22.02876472382295248, 15.47207198241065029, 68.84999999999999432 ) ) ;
#3476 = CARTESIAN_POINT ( 'NONE',  ( -0.05918829504999999908, 10.97290950744599947, 63.54999999999999716 ) ) ;
#3477 = ADVANCED_FACE ( 'NONE', ( #5837 ), #397, .T. ) ;
#3478 = FACE_OUTER_BOUND ( 'NONE', #7672, .T. ) ;
#3479 = SHAPE_REPRESENTATION_RELATIONSHIP ( 'NONE' , 'NONE' ,  #11399, #6247 ) ;
#3480 = AXIS2_PLACEMENT_3D ( 'NONE', #11448, #10542, #7103 ) ;
#3481 = EDGE_LOOP ( 'NONE', ( #13585, #6359, #8115, #13699 ) ) ;
#3482 = ORIENTED_EDGE ( 'NONE', *, *, #13758, .F. ) ;
#3483 = DIRECTION ( 'NONE',  ( -0.6615960714621564875, 0.7498604124941129490, 0.000000000000000000 ) ) ;
#3484 = ORIENTED_EDGE ( 'NONE', *, *, #12002, .F. ) ;
#3485 = CARTESIAN_POINT ( 'NONE',  ( -25.73489962141550080, -4.139534227248430120, 57.54999999999999716 ) ) ;
#3486 = ADVANCED_FACE ( 'NONE', ( #2455, #5899 ), #13181, .F. ) ;
#3487 = FACE_OUTER_BOUND ( 'NONE', #395, .T. ) ;
#3488 = DIRECTION ( 'NONE',  ( -1.000000000000000000, 0.000000000000000000, 0.000000000000000000 ) ) ;
#3489 = DIRECTION ( 'NONE',  ( 0.000000000000000000, 0.000000000000000000, 1.000000000000000000 ) ) ;
#3490 = LINE ( 'NONE', #5771, #6058 ) ;
#3491 = ORIENTED_EDGE ( 'NONE', *, *, #8319, .F. ) ;
#3492 = CYLINDRICAL_SURFACE ( 'NONE', #10668, 8.395833332999997012 ) ;
#3493 = DIRECTION ( 'NONE',  ( 0.000000000000000000, 0.000000000000000000, 1.000000000000000000 ) ) ;
#3494 = AXIS2_PLACEMENT_3D ( 'NONE', #12476, #13514, #12615 ) ;
#3495 = DIRECTION ( 'NONE',  ( 1.000000000000000000, 0.000000000000000000, 0.000000000000000000 ) ) ;
#3496 = DIRECTION ( 'NONE',  ( 1.000000000000000000, 0.000000000000000000, -0.000000000000000000 ) ) ;
#3497 = EDGE_CURVE ( 'NONE', #6884, #5387, #7565, .T. ) ;
#3498 = CIRCLE ( 'NONE', #5040, 16.99999999999999645 ) ;
#3499 = ORIENTED_EDGE ( 'NONE', *, *, #2064, .F. ) ;
#3500 = CARTESIAN_POINT ( 'NONE',  ( -18.05918829504999934, 30.47290950744599769, 57.35000000000000142 ) ) ;
#3502 = ORIENTED_EDGE ( 'NONE', *, *, #6345, .T. ) ;
#3501 = ADVANCED_FACE ( 'NONE', ( #4738, #4869 ), #10184, .F. ) ;
#3503 = DIRECTION ( 'NONE',  ( -0.6615960714621564875, 0.7498604124941129490, 0.000000000000000000 ) ) ;
#3504 = CARTESIAN_POINT ( 'NONE',  ( -18.05918829504999934, 10.97290950744599947, 57.35000000000000142 ) ) ;
#3505 = CARTESIAN_POINT ( 'NONE',  ( 112.1804561881462945, 85.78908161011133870, 0.7500000000000006661 ) ) ;
#3506 = DIRECTION ( 'NONE',  ( -0.4678190685372686231, 0.5302313826179265721, 0.7071067811865505703 ) ) ;
#3507 = DIRECTION ( 'NONE',  ( 0.6615960714621574867, -0.7498604124941119498, 0.000000000000000000 ) ) ;
#3508 = AXIS2_PLACEMENT_3D ( 'NONE', #9288, #4063, #13476 ) ;
#3509 = EDGE_CURVE ( 'NONE', #9587, #8944, #3358, .T. ) ;
#3510 = LINE ( 'NONE', #2551, #7346 ) ;
#3511 = ORIENTED_EDGE ( 'NONE', *, *, #5834, .T. ) ;
#3512 = VERTEX_POINT ( 'NONE', #1585 ) ;
#3513 = ORIENTED_EDGE ( 'NONE', *, *, #5497, .T. ) ;
#3514 = CARTESIAN_POINT ( 'NONE',  ( 24.03999999999999915, 2.944050905150237001E-15, 0.000000000000000000 ) ) ;
#3515 = ORIENTED_EDGE ( 'NONE', *, *, #1602, .T. ) ;
#3516 = ORIENTED_EDGE ( 'NONE', *, *, #12993, .F. ) ;
#3517 = VECTOR ( 'NONE', #7581, 1000.000000000000000 ) ;
#3518 = ORIENTED_EDGE ( 'NONE', *, *, #7957, .F. ) ;
#3519 = EDGE_LOOP ( 'NONE', ( #10606, #5170, #10765, #6921 ) ) ;
#3520 = DIRECTION ( 'NONE',  ( -0.6615960714621569316, 0.7498604124941123938, 0.000000000000000000 ) ) ;
#3521 = CARTESIAN_POINT ( 'NONE',  ( 134.6356359024541973, 108.9054980190242503, 20.00000000000000000 ) ) ;
#3522 = ORIENTED_EDGE ( 'NONE', *, *, #2424, .F. ) ;
#3523 = CYLINDRICAL_SURFACE ( 'NONE', #2744, 6.850000000000002309 ) ;
#3524 = CARTESIAN_POINT ( 'NONE',  ( 68.49370948373500312, 75.03908161011133870, 19.25000000000000000 ) ) ;
#3525 = CARTESIAN_POINT ( 'NONE',  ( -25.73489962141544751, -4.139534227248430120, 57.35000000000000142 ) ) ;
#3526 = EDGE_CURVE ( 'NONE', #4562, #12584, #10967, .T. ) ;
#3527 = DIRECTION ( 'NONE',  ( 1.000000000000000000, 0.000000000000000000, 0.000000000000000000 ) ) ;
#3528 = VECTOR ( 'NONE', #728, 1000.000000000000000 ) ;
#3529 = CIRCLE ( 'NONE', #6414, 4.250000000000003553 ) ;
#3530 = VECTOR ( 'NONE', #8695, 1000.000000000000000 ) ;
#3531 = EDGE_CURVE ( 'NONE', #4189, #3713, #6014, .T. ) ;
#3532 = ORIENTED_EDGE ( 'NONE', *, *, #10071, .F. ) ;
#3533 = VERTEX_POINT ( 'NONE', #10049 ) ;
#3534 = LINE ( 'NONE', #2572, #11967 ) ;
#3535 = ORIENTED_EDGE ( 'NONE', *, *, #9694, .F. ) ;
#3536 = CIRCLE ( 'NONE', #2880, 33.00000000000000000 ) ;
#3537 = PRESENTATION_STYLE_ASSIGNMENT (( #12443 ) ) ;
#3538 = VECTOR ( 'NONE', #8912, 1000.000000000000000 ) ;
#3539 = VECTOR ( 'NONE', #13114, 1000.000000000000000 ) ;
#3540 = FILL_AREA_STYLE_COLOUR ( '', #3974 ) ;
#3541 = CARTESIAN_POINT ( 'NONE',  ( -20.59415145364857835, 30.22157476193357439, 60.60836344892124572 ) ) ;
#3542 = SURFACE_STYLE_FILL_AREA ( #2643 ) ;
#3543 = VERTEX_POINT ( 'NONE', #12140 ) ;
#3544 = DIRECTION ( 'NONE',  ( 1.000000000000000000, 0.000000000000000000, 0.000000000000000000 ) ) ;
#3545 = CARTESIAN_POINT ( 'NONE',  ( -18.05918829504999934, 10.97290950744599947, 12.50000000000000000 ) ) ;
#3546 = DIRECTION ( 'NONE',  ( 0.4528443260392608916, 0.8915896008669279560, 0.000000000000000000 ) ) ;
#3547 = DIRECTION ( 'NONE',  ( 1.000000000000000000, 0.000000000000000000, 0.000000000000000000 ) ) ;
#3548 = CARTESIAN_POINT ( 'NONE',  ( 0.000000000000000000, 0.000000000000000000, 0.000000000000000000 ) ) ;
#3549 = ORIENTED_EDGE ( 'NONE', *, *, #10332, .F. ) ;
#3550 = EDGE_CURVE ( 'NONE', #5721, #1952, #7129, .T. ) ;
#3551 = CIRCLE ( 'NONE', #3109, 2.000000000000001776 ) ;
#3552 = CIRCLE ( 'NONE', #13571, 6.049999999999999822 ) ;
#3553 = EDGE_CURVE ( 'NONE', #8944, #1263, #1381, .T. ) ;
#3554 = CIRCLE ( 'NONE', #1536, 7.618085573000000110 ) ;
#3555 = ORIENTED_EDGE ( 'NONE', *, *, #767, .T. ) ;
#3556 = DIRECTION ( 'NONE',  ( 1.000000000000000000, 0.000000000000000000, 0.000000000000000000 ) ) ;
#3557 = CARTESIAN_POINT ( 'NONE',  ( -12.00918829504999863, 10.97290950744599947, 14.00000000000000000 ) ) ;
#3558 = ORIENTED_EDGE ( 'NONE', *, *, #5948, .T. ) ;
#3559 = CARTESIAN_POINT ( 'NONE',  ( -12.00000000000000000, -2.500000000000000444, 0.000000000000000000 ) ) ;
#3560 = EDGE_LOOP ( 'NONE', ( #8901, #2915 ) ) ;
#3561 = DIRECTION ( 'NONE',  ( 0.000000000000000000, 0.000000000000000000, -1.000000000000000000 ) ) ;
#3562 = PRODUCT_RELATED_PRODUCT_CATEGORY ( 'part', '', ( #12935 ) ) ;
#3563 = DIRECTION ( 'NONE',  ( -0.000000000000000000, 1.000000000000000000, -0.000000000000000000 ) ) ;
#3564 = DIRECTION ( 'NONE',  ( -1.000000000000000000, 0.000000000000000000, 0.000000000000000000 ) ) ;
#3565 = AXIS2_PLACEMENT_3D ( 'NONE', #5328, #31, #10721 ) ;
#3566 = FACE_OUTER_BOUND ( 'NONE', #7758, .T. ) ;
#3567 = CIRCLE ( 'NONE', #7313, 0.7500000000000006661 ) ;
#3568 = CARTESIAN_POINT ( 'NONE',  ( -35.05918829505000645, 10.97290950744599947, 57.35000000000000142 ) ) ;
#3569 = CARTESIAN_POINT ( 'NONE',  ( -35.05918829505000645, -6.027090492554000534, 10.00000000000000000 ) ) ;
#3570 = CONICAL_SURFACE ( 'NONE', #11362, 2.500000000000000000, 0.7853981633974532750 ) ;
#3571 = LINE ( 'NONE', #13257, #1754 ) ;
#3572 = EDGE_CURVE ( 'NONE', #952, #533, #13310, .T. ) ;
#3573 = ADVANCED_FACE ( 'NONE', ( #12202 ), #1103, .T. ) ;
#3574 = EDGE_LOOP ( 'NONE', ( #6516, #2015 ) ) ;
#3575 = AXIS2_PLACEMENT_3D ( 'NONE', #9248, #1775, #4010 ) ;
#3576 = DIRECTION ( 'NONE',  ( 1.000000000000000000, 0.000000000000000000, 0.000000000000000000 ) ) ;
#3577 = ORIENTED_EDGE ( 'NONE', *, *, #11226, .T. ) ;
#3578 = CIRCLE ( 'NONE', #6677, 17.50000000000000355 ) ;
#3579 = ORIENTED_EDGE ( 'NONE', *, *, #12811, .T. ) ;
#3580 = LINE ( 'NONE', #13329, #140 ) ;
#3581 = ADVANCED_FACE ( 'NONE', ( #9974 ), #6954, .T. ) ;
#3582 = CARTESIAN_POINT ( 'NONE',  ( -10.81426999815532852, 15.06602133594271820, -3.000000000000000000 ) ) ;
#3583 =( LENGTH_UNIT ( ) NAMED_UNIT ( * ) SI_UNIT ( .MILLI., .METRE. ) );
#3584 = CARTESIAN_POINT ( 'NONE',  ( 92.63563590245421153, 99.03908161011133870, 0.7500000000000006661 ) ) ;
#3585 = DIRECTION ( 'NONE',  ( -0.000000000000000000, -0.000000000000000000, 1.000000000000000000 ) ) ;
#3586 = LINE ( 'NONE', #7819, #674 ) ;
#3587 = ADVANCED_FACE ( 'NONE', ( #8923 ), #13105, .F. ) ;
#3588 = ORIENTED_EDGE ( 'NONE', *, *, #8167, .T. ) ;
#3589 = CARTESIAN_POINT ( 'NONE',  ( -16.66803132855381619, 30.31858837286686637, 61.40807488358109367 ) ) ;
#3590 = VERTEX_POINT ( 'NONE', #4797 ) ;
#3591 = ORIENTED_EDGE ( 'NONE', *, *, #1120, .T. ) ;
#3592 = EDGE_CURVE ( 'NONE', #3770, #4357, #4258, .T. ) ;
#3593 = VECTOR ( 'NONE', #7863, 1000.000000000000000 ) ;
#3594 = PRODUCT_DEFINITION_SHAPE ( 'NONE', 'NONE',  #13816 ) ;
#3595 = VERTEX_POINT ( 'NONE', #1651 ) ;
#3596 = VECTOR ( 'NONE', #4403, 1000.000000000000000 ) ;
#3597 = AXIS2_PLACEMENT_3D ( 'NONE', #5042, #10358, #10162 ) ;
#3598 = AXIS2_PLACEMENT_3D ( 'NONE', #9773, #197, #679 ) ;
#3599 = CARTESIAN_POINT ( 'NONE',  ( -18.05918829505001355, 3.364325185446006117, 61.98378871700002435 ) ) ;
#3600 = DIRECTION ( 'NONE',  ( -0.4678190685372707325, 0.5302313826179287926, 0.7071067811865475727 ) ) ;
#3601 = ORIENTED_EDGE ( 'NONE', *, *, #10615, .F. ) ;
#3602 = FACE_OUTER_BOUND ( 'NONE', #839, .T. ) ;
#3603 = CARTESIAN_POINT ( 'NONE',  ( 134.8856359024541973, 108.6554980190242503, 23.00000000000000000 ) ) ;
#3604 = FACE_OUTER_BOUND ( 'NONE', #11042, .T. ) ;
#3605 = CARTESIAN_POINT ( 'NONE',  ( 68.49370948373500312, 75.03908161011133870, 0.7500000000000006661 ) ) ;
#3606 = AXIS2_PLACEMENT_3D ( 'NONE', #4445, #5930, #13348 ) ;
#3607 = AXIS2_PLACEMENT_3D ( 'NONE', #57, #12979, #7498 ) ;
#3608 = APPLICATION_CONTEXT ( 'automotive_design' ) ;
#3609 = VERTEX_POINT ( 'NONE', #3557 ) ;
#3610 = VERTEX_POINT ( 'NONE', #7788 ) ;
#3611 = EDGE_CURVE ( 'NONE', #8025, #1567, #2523, .T. ) ;
#3612 = CARTESIAN_POINT ( 'NONE',  ( 8.000000000000001776, 2.000000000000000000, -65.00000000000000000 ) ) ;
#3613 = VERTEX_POINT ( 'NONE', #10051 ) ;
#3614 = ORIENTED_EDGE ( 'NONE', *, *, #4766, .F. ) ;
#3615 = CARTESIAN_POINT ( 'NONE',  ( -21.25220226754673547, 30.13979931660498579, 54.95335517942023529 ) ) ;
#3616 = VECTOR ( 'NONE', #4618, 1000.000000000000000 ) ;
#3617 = AXIS2_PLACEMENT_3D ( 'NONE', #6240, #10513, #9256 ) ;
#3618 =( NAMED_UNIT ( * ) SI_UNIT ( $, .STERADIAN. ) SOLID_ANGLE_UNIT ( ) );
#3619 = DIRECTION ( 'NONE',  ( 0.000000000000000000, 0.000000000000000000, -1.000000000000000000 ) ) ;
#3620 = VECTOR ( 'NONE', #6750, 1000.000000000000000 ) ;
#3621 = PLANE ( 'NONE',  #6436 ) ;
#3622 = CARTESIAN_POINT ( 'NONE',  ( 0.000000000000000000, -17.50000000000000000, 6.000000000000000888 ) ) ;
#3623 = FACE_OUTER_BOUND ( 'NONE', #476, .T. ) ;
#3624 = SHAPE_REPRESENTATION_RELATIONSHIP ( 'NONE' , 'NONE' ,  #2236, #7898 ) ;
#3625 = AXIS2_PLACEMENT_3D ( 'NONE', #12369, #10402, #765 ) ;
#3626 = ORIENTED_EDGE ( 'NONE', *, *, #5948, .F. ) ;
#3627 = VERTEX_POINT ( 'NONE', #3559 ) ;
#3628 = VERTEX_POINT ( 'NONE', #10972 ) ;
#3629 = DIRECTION ( 'NONE',  ( -0.000000000000000000, -0.000000000000000000, -1.000000000000000000 ) ) ;
#3630 = CARTESIAN_POINT ( 'NONE',  ( -18.05918829504999934, 10.97290950744599947, 63.35000000000000142 ) ) ;
#3631 = DIRECTION ( 'NONE',  ( 1.000000000000000000, -0.000000000000000000, 0.000000000000000000 ) ) ;
#3632 = FILL_AREA_STYLE_COLOUR ( '', #1501 ) ;
#3633 = DIRECTION ( 'NONE',  ( 0.7071067811865500152, 0.7071067811865451302, 0.000000000000000000 ) ) ;
#3634 = DIRECTION ( 'NONE',  ( 1.000000000000000000, 0.000000000000000000, 0.000000000000000000 ) ) ;
#3635 = FACE_OUTER_BOUND ( 'NONE', #6512, .T. ) ;
#3636 = EDGE_CURVE ( 'NONE', #6678, #12858, #13108, .T. ) ;
#3637 = DIRECTION ( 'NONE',  ( 0.000000000000000000, 0.000000000000000000, -1.000000000000000000 ) ) ;
#3638 = CARTESIAN_POINT ( 'NONE',  ( -10.25088531517539714, 30.80589556422609832, 5.250000000000000000 ) ) ;
#3639 = ADVANCED_FACE ( 'NONE', ( #5765 ), #12068, .F. ) ;
#3640 = DIRECTION ( 'NONE',  ( 0.000000000000000000, 0.000000000000000000, 1.000000000000000000 ) ) ;
#3641 = AXIS2_PLACEMENT_3D ( 'NONE', #12885, #8423, #1020 ) ;
#3642 = DIRECTION ( 'NONE',  ( 0.000000000000000000, -1.000000000000000000, 0.000000000000000000 ) ) ;
#3643 = CARTESIAN_POINT ( 'NONE',  ( 44.94629607423406270, 112.2890816101113387, 0.000000000000000000 ) ) ;
#3644 = VECTOR ( 'NONE', #13772, 1000.000000000000000 ) ;
#3645 = CARTESIAN_POINT ( 'NONE',  ( -32.05918829504999934, 27.97290950744599769, 0.000000000000000000 ) ) ;
#3646 = ORIENTED_EDGE ( 'NONE', *, *, #8395, .T. ) ;
#3647 = VERTEX_POINT ( 'NONE', #12974 ) ;
#3648 = DIRECTION ( 'NONE',  ( 0.000000000000000000, 0.000000000000000000, 1.000000000000000000 ) ) ;
#3649 = DIRECTION ( 'NONE',  ( 0.000000000000000000, 0.000000000000000000, 1.000000000000000000 ) ) ;
#3650 = CARTESIAN_POINT ( 'NONE',  ( -35.05918829505000645, -6.027090492554000534, 68.85549045786049760 ) ) ;
#3651 = DIRECTION ( 'NONE',  ( 0.000000000000000000, 0.000000000000000000, -1.000000000000000000 ) ) ;
#3652 = EDGE_CURVE ( 'NONE', #1569, #3713, #9853, .T. ) ;
#3653 = CARTESIAN_POINT ( 'NONE',  ( 141.8856359024541973, 99.03908161011133870, 19.25000000000000000 ) ) ;
#3654 = FACE_OUTER_BOUND ( 'NONE', #11397, .T. ) ;
#3655 = AXIS2_PLACEMENT_3D ( 'NONE', #8643, #9311, #5492 ) ;
#3656 = EDGE_CURVE ( 'NONE', #9517, #1552, #3422, .T. ) ;
#3657 = ORIENTED_EDGE ( 'NONE', *, *, #507, .F. ) ;
#3658 = DIRECTION ( 'NONE',  ( 0.000000000000000000, 0.000000000000000000, 1.000000000000000000 ) ) ;
#3659 = ORIENTED_EDGE ( 'NONE', *, *, #5188, .F. ) ;
#3660 = EDGE_LOOP ( 'NONE', ( #9021, #12465, #5916, #10909 ) ) ;
#3661 = ORIENTED_EDGE ( 'NONE', *, *, #11608, .T. ) ;
#3662 = AXIS2_PLACEMENT_3D ( 'NONE', #7027, #8152, #13594 ) ;
#3663 = ORIENTED_EDGE ( 'NONE', *, *, #6718, .F. ) ;
#3664 = CARTESIAN_POINT ( 'NONE',  ( 3.500000000000001776, 2.499999999999999556, -65.00000000000000000 ) ) ;
#3665 = CARTESIAN_POINT ( 'NONE',  ( 141.8856359024541973, 111.0390816101113103, 20.00000000000000000 ) ) ;
#3666 = EDGE_CURVE ( 'NONE', #11864, #9880, #2526, .T. ) ;
#3667 = EDGE_LOOP ( 'NONE', ( #819, #8424 ) ) ;
#3668 = DIRECTION ( 'NONE',  ( 0.000000000000000000, 0.000000000000000000, -1.000000000000000000 ) ) ;
#3669 = CARTESIAN_POINT ( 'NONE',  ( 103.4499059006094512, 83.97306027416853169, 20.00000000000000000 ) ) ;
#3670 = FACE_OUTER_BOUND ( 'NONE', #1712, .T. ) ;
#3671 = DIRECTION ( 'NONE',  ( 1.000000000000000000, 0.000000000000000000, 0.000000000000000000 ) ) ;
#3672 = EDGE_CURVE ( 'NONE', #10592, #9852, #1445, .T. ) ;
#3673 = ORIENTED_EDGE ( 'NONE', *, *, #523, .F. ) ;
#3674 = VERTEX_POINT ( 'NONE', #272 ) ;
#3675 = VERTEX_POINT ( 'NONE', #12142 ) ;
#3676 = CARTESIAN_POINT ( 'NONE',  ( 44.63563590245420443, 108.9054980190242503, 22.75000000000000000 ) ) ;
#3677 = ADVANCED_FACE ( 'NONE', ( #9975 ), #11931, .F. ) ;
#3678 = CARTESIAN_POINT ( 'NONE',  ( -21.66168941035279971, 30.07924626547317715, 58.82219030866655629 ) ) ;
#3679 =( NAMED_UNIT ( * ) SI_UNIT ( $, .STERADIAN. ) SOLID_ANGLE_UNIT ( ) );
#3680 = CARTESIAN_POINT ( 'NONE',  ( 140.1053058165642824, 85.56941169600125363, 0.000000000000000000 ) ) ;
#3681 = CARTESIAN_POINT ( 'NONE',  ( -10.78334210919089919, -7.245613863947199640, 68.85549045786049760 ) ) ;
#3682 = CARTESIAN_POINT ( 'NONE',  ( -9.663354962050000552, 10.97290950744599947, 60.04999999999999716 ) ) ;
#3683 = CARTESIAN_POINT ( 'NONE',  ( -21.29702522623070138, 4.598043861247458786, 64.85000000000000853 ) ) ;
#3684 = CARTESIAN_POINT ( 'NONE',  ( 0.000000000000000000, 0.000000000000000000, 0.000000000000000000 ) ) ;
#3685 = EDGE_CURVE ( 'NONE', #9992, #5932, #13184, .T. ) ;
#3686 = DIRECTION ( 'NONE',  ( 1.000000000000000000, 0.000000000000000000, 0.000000000000000000 ) ) ;
#3687 = CARTESIAN_POINT ( 'NONE',  ( -8.499999999999998224, 2.000000000000000000, 0.000000000000000000 ) ) ;
#3688 = LINE ( 'NONE', #3485, #1802 ) ;
#3689 = LINE ( 'NONE', #6686, #7276 ) ;
#3690 = CYLINDRICAL_SURFACE ( 'NONE', #8881, 1.999999999999991340 ) ;
#3691 = DIRECTION ( 'NONE',  ( -0.7071067811865451302, 0.7071067811865500152, 0.000000000000000000 ) ) ;
#3692 = CYLINDRICAL_SURFACE ( 'NONE', #9642, 0.7500000000000000000 ) ;
#3693 = CARTESIAN_POINT ( 'NONE',  ( 3.940811704950003325, 32.97290950744599769, 10.00000000000000000 ) ) ;
#3694 = DIRECTION ( 'NONE',  ( -0.9496839325805427334, -0.3132098788326367345, 0.000000000000000000 ) ) ;
#3695 = DIRECTION ( 'NONE',  ( -1.000000000000000000, 0.000000000000000000, 0.000000000000000000 ) ) ;
#3696 = DIRECTION ( 'NONE',  ( 0.000000000000000000, 0.000000000000000000, 1.000000000000000000 ) ) ;
#3697 = CARTESIAN_POINT ( 'NONE',  ( -12.00000000000000000, -2.500000000000000444, -65.00000000000000000 ) ) ;
#3698 = EDGE_CURVE ( 'NONE', #5985, #11975, #13043, .T. ) ;
#3699 = PRODUCT_DEFINITION_SHAPE ( 'NONE', 'NONE',  #10061 ) ;
#3700 = ORIENTED_EDGE ( 'NONE', *, *, #9319, .T. ) ;
#3701 = EDGE_CURVE ( 'NONE', #1587, #5576, #6610, .T. ) ;
#3702 = ORIENTED_EDGE ( 'NONE', *, *, #11265, .T. ) ;
#3703 = CYLINDRICAL_SURFACE ( 'NONE', #9266, 0.9499999999999995115 ) ;
#3704 = ORIENTED_EDGE ( 'NONE', *, *, #13261, .T. ) ;
#3705 = DIRECTION ( 'NONE',  ( -0.000000000000000000, -0.000000000000000000, 1.000000000000000000 ) ) ;
#3706 = AXIS2_PLACEMENT_3D ( 'NONE', #10377, #8351, #3003 ) ;
#3707 = CARTESIAN_POINT ( 'NONE',  ( -1.059188295049996231, -6.027090492554000534, 64.85000000000000853 ) ) ;
#3708 = DIRECTION ( 'NONE',  ( 0.000000000000000000, 0.000000000000000000, -1.000000000000000000 ) ) ;
#3709 = CARTESIAN_POINT ( 'NONE',  ( 16.45469220996245241, 1.832421873814834345, 0.000000000000000000 ) ) ;
#3710 = DIRECTION ( 'NONE',  ( 0.000000000000000000, 0.000000000000000000, 1.000000000000000000 ) ) ;
#3711 = DIRECTION ( 'NONE',  ( 0.000000000000000000, 0.000000000000000000, 1.000000000000000000 ) ) ;
#3712 = AXIS2_PLACEMENT_3D ( 'NONE', #12049, #4648, #5674 ) ;
#3713 = VERTEX_POINT ( 'NONE', #4595 ) ;
#3714 = EDGE_CURVE ( 'NONE', #5137, #12100, #3688, .T. ) ;
#3715 = ORIENTED_EDGE ( 'NONE', *, *, #10117, .F. ) ;
#3716 = CARTESIAN_POINT ( 'NONE',  ( -18.05918829504999934, 19.07290950615085023, 63.35000000000700027 ) ) ;
#3717 = AXIS2_PLACEMENT_3D ( 'NONE', #13489, #1362, #3867 ) ;
#3718 = ORIENTED_EDGE ( 'NONE', *, *, #10632, .F. ) ;
#3719 = ORIENTED_EDGE ( 'NONE', *, *, #1244, .F. ) ;
#3720 = ORIENTED_EDGE ( 'NONE', *, *, #12377, .F. ) ;
#3721 = PLANE ( 'NONE',  #12515 ) ;
#3722 = FACE_OUTER_BOUND ( 'NONE', #12896, .T. ) ;
#3723 = DIRECTION ( 'NONE',  ( 0.000000000000000000, 0.000000000000000000, -1.000000000000000000 ) ) ;
#3724 = COLOUR_RGB ( '', 0.40784314, 0.44705882, 0.49803922) ;
#3725 = CARTESIAN_POINT ( 'NONE',  ( -18.05918829504998868, 19.27290950775476475, 63.26715728756898471 ) ) ;
#3726 = EDGE_CURVE ( 'NONE', #12649, #3976, #1115, .T. ) ;
#3727 = DIRECTION ( 'NONE',  ( 0.000000000000000000, 0.000000000000000000, -1.000000000000000000 ) ) ;
#3728 = DIRECTION ( 'NONE',  ( -0.4528443260392610026, -0.8915896008669278450, 0.000000000000000000 ) ) ;
#3729 = DIRECTION ( 'NONE',  ( 0.000000000000000000, 0.000000000000000000, 1.000000000000000000 ) ) ;
#3730 =( BOUNDED_CURVE ( )  B_SPLINE_CURVE ( 3, ( #11774, #9547, #9690, #106 ),
 .UNSPECIFIED., .F., .F. ) 
 B_SPLINE_CURVE_WITH_KNOTS ( ( 4, 4 ),
 ( 0.000000000000000000, 1.570796326794896558 ),
 .UNSPECIFIED. ) 
 CURVE ( )  GEOMETRIC_REPRESENTATION_ITEM ( )  RATIONAL_B_SPLINE_CURVE ( ( 1.000000000000000000, 0.8047378541243649375, 0.8047378541243649375, 1.000000000000000000 ) ) 
 REPRESENTATION_ITEM ( '' )  );
#3731 = CIRCLE ( 'NONE', #11531, 1.999999999999991340 ) ;
#3732 = ADVANCED_FACE ( 'NONE', ( #9764 ), #477, .T. ) ;
#3733 = AXIS2_PLACEMENT_3D ( 'NONE', #6759, #13185, #5901 ) ;
#3734 = ORIENTED_EDGE ( 'NONE', *, *, #9533, .F. ) ;
#3735 = EDGE_LOOP ( 'NONE', ( #5057, #856, #207, #21 ) ) ;
#3736 = DIRECTION ( 'NONE',  ( 0.000000000000000000, 0.000000000000000000, 1.000000000000000000 ) ) ;
#3737 = ORIENTED_EDGE ( 'NONE', *, *, #12767, .F. ) ;
#3738 = SURFACE_SIDE_STYLE ('',( #2574 ) ) ;
#3739 = EDGE_CURVE ( 'NONE', #10924, #2221, #5484, .T. ) ;
#3740 = CARTESIAN_POINT ( 'NONE',  ( -21.43229256600465149, 30.11415384995645894, 55.29115902660671367 ) ) ;
#3741 = VECTOR ( 'NONE', #2996, 1000.000000000000000 ) ;
#3742 = DIRECTION ( 'NONE',  ( 0.000000000000000000, 0.000000000000000000, 1.000000000000000000 ) ) ;
#3743 = CARTESIAN_POINT ( 'NONE',  ( 50.63563590245420443, 103.9054980190242361, 22.89644660940672694 ) ) ;
#3744 = PLANE ( 'NONE',  #4196 ) ;
#3745 = CARTESIAN_POINT ( 'NONE',  ( -0.05918829504999999908, 10.97290950744599947, 63.45000000000000284 ) ) ;
#3746 = VECTOR ( 'NONE', #6669, 1000.000000000000000 ) ;
#3747 = DIRECTION ( 'NONE',  ( 0.000000000000000000, 0.000000000000000000, 1.000000000000000000 ) ) ;
#3748 =( NAMED_UNIT ( * ) SI_UNIT ( $, .STERADIAN. ) SOLID_ANGLE_UNIT ( ) );
#3749 = ADVANCED_FACE ( 'NONE', ( #5560 ), #11998, .F. ) ;
#3750 = AXIS2_PLACEMENT_3D ( 'NONE', #1612, #3392, #3460 ) ;
#3751 = AXIS2_PLACEMENT_3D ( 'NONE', #1512, #9978, #12070 ) ;
#3752 = VECTOR ( 'NONE', #3456, 1000.000000000000000 ) ;
#3753 = CARTESIAN_POINT ( 'NONE',  ( -12.00000000000000000, 2.500000000000000000, 0.000000000000000000 ) ) ;
#3754 = DIRECTION ( 'NONE',  ( 1.000000000000000000, 0.000000000000000000, 0.000000000000000000 ) ) ;
#3755 = CARTESIAN_POINT ( 'NONE',  ( -5.173045190668890569, -15.68519459986890041, 17.25000000000000000 ) ) ;
#3756 = SURFACE_SIDE_STYLE ('',( #5696 ) ) ;
#3757 = ADVANCED_FACE ( 'NONE', ( #5633 ), #4706, .T. ) ;
#3758 = DIRECTION ( 'NONE',  ( 0.000000000000000000, 0.000000000000000000, 1.000000000000000000 ) ) ;
#3759 = ADVANCED_BREP_SHAPE_REPRESENTATION ( '', ( #9762, #6434 ), #4214 ) ;
#3760 = CYLINDRICAL_SURFACE ( 'NONE', #5801, 2.700000000000001066 ) ;
#3761 = DIRECTION ( 'NONE',  ( -0.000000000000000000, 1.000000000000000000, -0.000000000000000000 ) ) ;
#3762 = DIRECTION ( 'NONE',  ( -1.000000000000000000, 0.000000000000000000, 0.000000000000000000 ) ) ;
#3763 = LINE ( 'NONE', #4602, #1069 ) ;
#3764 = CARTESIAN_POINT ( 'NONE',  ( -18.05918829504999934, 10.97290950744599947, 27.09999999999999787 ) ) ;
#3765 = PLANE ( 'NONE',  #5420 ) ;
#3766 = CARTESIAN_POINT ( 'NONE',  ( 4.599650328638321461, 8.500000000000001776, 7.878124499050794149 ) ) ;
#3767 = CIRCLE ( 'NONE', #3750, 10.74999999999999645 ) ;
#3768 = VECTOR ( 'NONE', #2338, 1000.000000000000000 ) ;
#3769 = CIRCLE ( 'NONE', #5980, 6.000000000000000888 ) ;
#3770 = VERTEX_POINT ( 'NONE', #6047 ) ;
#3771 = ORIENTED_EDGE ( 'NONE', *, *, #753, .F. ) ;
#3772 = CARTESIAN_POINT ( 'NONE',  ( -30.48673169511680214, 10.97290950744599947, 68.85549045786049760 ) ) ;
#3773 = AXIS2_PLACEMENT_3D ( 'NONE', #4607, #11240, #9062 ) ;
#3774 = VECTOR ( 'NONE', #9752, 1000.000000000000000 ) ;
#3775 = VERTEX_POINT ( 'NONE', #7161 ) ;
#3776 = CARTESIAN_POINT ( 'NONE',  ( 75.58559257550551536, 82.08927268643400055, 20.00000000000000000 ) ) ;
#3777 = TOROIDAL_SURFACE ( 'NONE', #2465, 10.75000000000000000, 0.7500000000000000000 ) ;
#3778 = ADVANCED_FACE ( 'NONE', ( #7019 ), #7803, .T. ) ;
#3779 = FACE_OUTER_BOUND ( 'NONE', #12319, .T. ) ;
#3780 = CARTESIAN_POINT ( 'NONE',  ( -5.809188295050001116, -6.027090492554000534, 68.85549045786049760 ) ) ;
#3781 = DIRECTION ( 'NONE',  ( 0.000000000000000000, 0.000000000000000000, -1.000000000000000000 ) ) ;
#3782 = APPLICATION_CONTEXT ( 'automotive_design' ) ;
#3783 = FACE_OUTER_BOUND ( 'NONE', #8065, .T. ) ;
#3784 = DIRECTION ( 'NONE',  ( 0.000000000000000000, 0.000000000000000000, -1.000000000000000000 ) ) ;
#3785 = AXIS2_PLACEMENT_3D ( 'NONE', #6227, #7258, #8332 ) ;
#3786 = AXIS2_PLACEMENT_3D ( 'NONE', #1709, #1791, #10440 ) ;
#3787 = ORIENTED_EDGE ( 'NONE', *, *, #10166, .T. ) ;
#3788 = DIRECTION ( 'NONE',  ( -0.6615960714621568206, 0.7498604124941127269, 0.000000000000000000 ) ) ;
#3789 = ORIENTED_EDGE ( 'NONE', *, *, #5785, .T. ) ;
#3790 = FACE_OUTER_BOUND ( 'NONE', #3448, .T. ) ;
#3791 = ORIENTED_EDGE ( 'NONE', *, *, #9309, .T. ) ;
#3792 = DIRECTION ( 'NONE',  ( 0.000000000000000000, 0.000000000000000000, 1.000000000000000000 ) ) ;
#3793 = VERTEX_POINT ( 'NONE', #7087 ) ;
#3794 = CARTESIAN_POINT ( 'NONE',  ( 0.000000000000000000, 0.000000000000000000, 0.000000000000000000 ) ) ;
#3795 = DIRECTION ( 'NONE',  ( 0.000000000000000000, 0.000000000000000000, -1.000000000000000000 ) ) ;
#3796 = VERTEX_POINT ( 'NONE', #2731 ) ;
#3797 = CARTESIAN_POINT ( 'NONE',  ( -10.25088531517540069, -8.860076549334102936, 17.25000000000000000 ) ) ;
#3798 = VECTOR ( 'NONE', #5693, 1000.000000000000000 ) ;
#3799 = CARTESIAN_POINT ( 'NONE',  ( -7.241070169793059286, -7.867426463707969830, 5.250000000000000000 ) ) ;
#3800 = AXIS2_PLACEMENT_3D ( 'NONE', #9404, #4927, #5055 ) ;
#3801 = EDGE_CURVE ( 'NONE', #11171, #7594, #11387, .T. ) ;
#3802 = CARTESIAN_POINT ( 'NONE',  ( -35.05918829505000645, -6.027090492554000534, 58.85000000000000142 ) ) ;
#3803 = EDGE_CURVE ( 'NONE', #7944, #4071, #5900, .T. ) ;
#3804 = DIRECTION ( 'NONE',  ( 0.000000000000000000, 0.000000000000000000, -1.000000000000000000 ) ) ;
#3805 = AXIS2_PLACEMENT_3D ( 'NONE', #5839, #2936, #6108 ) ;
#3806 = CIRCLE ( 'NONE', #3359, 0.7499999999999966693 ) ;
#3807 = AXIS2_PLACEMENT_3D ( 'NONE', #1646, #13373, #9119 ) ;
#3808 = TOROIDAL_SURFACE ( 'NONE', #4710, 23.29163056034262169, 0.7500000000000000000 ) ;
#3809 = ORIENTED_EDGE ( 'NONE', *, *, #5497, .F. ) ;
#3810 = EDGE_LOOP ( 'NONE', ( #4497, #4575, #9698, #12334 ) ) ;
#3811 = ORIENTED_EDGE ( 'NONE', *, *, #9817, .T. ) ;
#3812 = CARTESIAN_POINT ( 'NONE',  ( 142.6356359024541973, 87.03908161011133870, 19.25000000000000000 ) ) ;
#3813 = CARTESIAN_POINT ( 'NONE',  ( -21.53500198183446557, 30.09884447264290941, 59.17606103016743191 ) ) ;
#3814 = CARTESIAN_POINT ( 'NONE',  ( 16.08092853089229024, 4.500000000000000000, -9.237812082545193704 ) ) ;
#3815 = EDGE_CURVE ( 'NONE', #6126, #898, #805, .T. ) ;
#3816 = CARTESIAN_POINT ( 'NONE',  ( 6.000000000000000888, 0.000000000000000000, 7.000000000000000000 ) ) ;
#3817 = CARTESIAN_POINT ( 'NONE',  ( -13.40033457972183939, -4.525318844826149878, 63.45000000000000284 ) ) ;
#3818 = ADVANCED_FACE ( 'NONE', ( #9130 ), #7344, .T. ) ;
#3819 = FACE_OUTER_BOUND ( 'NONE', #9545, .T. ) ;
#3820 = AXIS2_PLACEMENT_3D ( 'NONE', #7220, #3006, #5266 ) ;
#3821 =( BOUNDED_CURVE ( )  B_SPLINE_CURVE ( 3, ( #4320, #12763, #3275, #4452 ),
 .UNSPECIFIED., .F., .F. ) 
 B_SPLINE_CURVE_WITH_KNOTS ( ( 4, 4 ),
 ( 0.000000000000000000, 1.570796326794896558 ),
 .UNSPECIFIED. ) 
 CURVE ( )  GEOMETRIC_REPRESENTATION_ITEM ( )  RATIONAL_B_SPLINE_CURVE ( ( 1.000000000000000000, 0.8047378541243649375, 0.8047378541243649375, 1.000000000000000000 ) ) 
 REPRESENTATION_ITEM ( '' )  );
#3822 = AXIS2_PLACEMENT_3D ( 'NONE', #4464, #3284, #119 ) ;
#3823 = DIRECTION ( 'NONE',  ( 4.597850203645602824E-29, -6.780744947014009727E-15, 1.000000000000000000 ) ) ;
#3824 = EDGE_LOOP ( 'NONE', ( #7924, #7401, #454, #337 ) ) ;
#3825 = CIRCLE ( 'NONE', #2049, 20.00000000000000000 ) ;
#3826 = EDGE_CURVE ( 'NONE', #9617, #13769, #2269, .T. ) ;
#3827 = CIRCLE ( 'NONE', #2726, 17.66282263685195275 ) ;
#3828 = DIRECTION ( 'NONE',  ( -1.000000000000000000, 0.000000000000000000, 0.000000000000000000 ) ) ;
#3829 = VECTOR ( 'NONE', #10261, 1000.000000000000000 ) ;
#3830 = CARTESIAN_POINT ( 'NONE',  ( 0.04028432657539327000, 0.000000000000000000, -18.54539866546729243 ) ) ;
#3831 = AXIS2_PLACEMENT_3D ( 'NONE', #6585, #10860, #12944 ) ;
#3832 = ORIENTED_EDGE ( 'NONE', *, *, #13306, .T. ) ;
#3833 = LINE ( 'NONE', #5067, #11836 ) ;
#3834 = DIRECTION ( 'NONE',  ( 1.000000000000000000, 0.000000000000000000, 0.000000000000000000 ) ) ;
#3835 = DIRECTION ( 'NONE',  ( 0.000000000000000000, 0.000000000000000000, 1.000000000000000000 ) ) ;
#3836 = CARTESIAN_POINT ( 'NONE',  ( -36.05918829505000645, 10.97290950744599947, 63.54999999999999716 ) ) ;
#3837 = CARTESIAN_POINT ( 'NONE',  ( 123.1053058165644671, 129.5087515242213669, 20.00000000000000000 ) ) ;
#3838 = DIRECTION ( 'NONE',  ( -1.000000000000000000, 0.000000000000000000, 0.000000000000000000 ) ) ;
#3839 = CARTESIAN_POINT ( 'NONE',  ( 0.000000000000000000, 4.500000000000000000, 0.000000000000000000 ) ) ;
#3840 = CYLINDRICAL_SURFACE ( 'NONE', #11, 0.2500000000000002220 ) ;
#3841 = EDGE_CURVE ( 'NONE', #194, #2105, #10282, .T. ) ;
#3842 = FACE_BOUND ( 'NONE', #4628, .T. ) ;
#3843 = DIRECTION ( 'NONE',  ( -1.000000000000000000, 0.000000000000000000, 0.000000000000000000 ) ) ;
#3844 = VECTOR ( 'NONE', #12900, 1000.000000000000000 ) ;
#3845 = CIRCLE ( 'NONE', #3396, 1.999999999999991340 ) ;
#3846 = CIRCLE ( 'NONE', #12059, 0.9499999999999995115 ) ;
#3847 = EDGE_CURVE ( 'NONE', #4952, #1042, #2658, .T. ) ;
#3848 = ORIENTED_EDGE ( 'NONE', *, *, #8265, .T. ) ;
#3849 = ORIENTED_EDGE ( 'NONE', *, *, #5686, .F. ) ;
#3850 = DIRECTION ( 'NONE',  ( 0.000000000000000000, 0.000000000000000000, 1.000000000000000000 ) ) ;
#3851 = ORIENTED_EDGE ( 'NONE', *, *, #9817, .F. ) ;
#3852 = DIRECTION ( 'NONE',  ( -1.000000000000000000, 0.000000000000000000, 0.000000000000000000 ) ) ;
#3853 = VECTOR ( 'NONE', #12690, 1000.000000000000000 ) ;
#3854 = CARTESIAN_POINT ( 'NONE',  ( -7.241070169793063727, -7.867426463707971607, 17.25000000000000000 ) ) ;
#3855 = CARTESIAN_POINT ( 'NONE',  ( 75.58559257550551536, 82.08927268643400055, 19.25000000000000000 ) ) ;
#3856 = EDGE_CURVE ( 'NONE', #10151, #1164, #8033, .T. ) ;
#3857 = DIRECTION ( 'NONE',  ( 0.000000000000000000, 0.000000000000000000, -1.000000000000000000 ) ) ;
#3858 = CYLINDRICAL_SURFACE ( 'NONE', #9145, 2.700000000000000178 ) ;
#3859 = DIRECTION ( 'NONE',  ( 0.6615960714621567096, -0.7498604124941127269, 0.000000000000000000 ) ) ;
#3860 = EDGE_CURVE ( 'NONE', #5017, #3252, #3833, .T. ) ;
#3861 = AXIS2_PLACEMENT_3D ( 'NONE', #10368, #727, #12265 ) ;
#3862 = ORIENTED_EDGE ( 'NONE', *, *, #10846, .T. ) ;
#3863 = EDGE_LOOP ( 'NONE', ( #3438, #2485, #13202, #6991 ) ) ;
#3864 = CARTESIAN_POINT ( 'NONE',  ( -15.88770235650742002, 30.25856101889280225, 60.93332845326816027 ) ) ;
#3865 = ORIENTED_EDGE ( 'NONE', *, *, #10743, .F. ) ;
#3866 = ORIENTED_EDGE ( 'NONE', *, *, #10802, .T. ) ;
#3867 = DIRECTION ( 'NONE',  ( 0.000000000000000000, 0.000000000000000000, 1.000000000000000000 ) ) ;
#3868 = CARTESIAN_POINT ( 'NONE',  ( -18.05918829358019906, 3.806800778008990083, 61.72253826514069885 ) ) ;
#3869 = ORIENTED_EDGE ( 'NONE', *, *, #5166, .F. ) ;
#3870 = CARTESIAN_POINT ( 'NONE',  ( -33.29928216905001648, 3.352862570445993562, 61.63595870799996845 ) ) ;
#3871 = FACE_OUTER_BOUND ( 'NONE', #12511, .T. ) ;
#3872 = VERTEX_POINT ( 'NONE', #8080 ) ;
#3873 = DIRECTION ( 'NONE',  ( 0.7071067811865382469, -0.7071067811865567876, 0.000000000000000000 ) ) ;
#3874 = VECTOR ( 'NONE', #2327, 1000.000000000000114 ) ;
#3875 = CARTESIAN_POINT ( 'NONE',  ( -25.86749127492454647, -8.860076549334127805, 17.25000000000000000 ) ) ;
#3876 = DIRECTION ( 'NONE',  ( -0.000000000000000000, -0.000000000000000000, -1.000000000000000000 ) ) ;
#3877 = DIRECTION ( 'NONE',  ( -0.000000000000000000, -0.000000000000000000, 1.000000000000000000 ) ) ;
#3878 = ORIENTED_EDGE ( 'NONE', *, *, #13017, .T. ) ;
#3879 = AXIS2_PLACEMENT_3D ( 'NONE', #12214, #13116, #10979 ) ;
#3880 = ORIENTED_EDGE ( 'NONE', *, *, #10237, .T. ) ;
#3881 = ADVANCED_FACE ( 'NONE', ( #8214 ), #1588, .T. ) ;
#3882 = ORIENTED_EDGE ( 'NONE', *, *, #3656, .F. ) ;
#3883 = EDGE_LOOP ( 'NONE', ( #10092, #9235, #13516, #431 ) ) ;
#3884 = DIRECTION ( 'NONE',  ( -1.000000000000000000, -0.000000000000000000, -0.000000000000000000 ) ) ;
#3885 = CARTESIAN_POINT ( 'NONE',  ( -19.81655147050198451, 30.29372715545316908, 61.21836758686404067 ) ) ;
#3886 = ORIENTED_EDGE ( 'NONE', *, *, #2363, .F. ) ;
#3887 = DIRECTION ( 'NONE',  ( 0.000000000000000000, 0.000000000000000000, 1.000000000000000000 ) ) ;
#3888 = CYLINDRICAL_SURFACE ( 'NONE', #9321, 0.5000000000000004441 ) ;
#3889 = FACE_OUTER_BOUND ( 'NONE', #618, .T. ) ;
#3890 = DIRECTION ( 'NONE',  ( 0.000000000000000000, 0.000000000000000000, 1.000000000000000000 ) ) ;
#3891 = ORIENTED_EDGE ( 'NONE', *, *, #7820, .T. ) ;
#3892 = ORIENTED_EDGE ( 'NONE', *, *, #4255, .F. ) ;
#3893 = EDGE_CURVE ( 'NONE', #898, #13375, #5967, .T. ) ;
#3894 = VERTEX_POINT ( 'NONE', #742 ) ;
#3895 = CARTESIAN_POINT ( 'NONE',  ( 68.49370948373500312, 123.0390816101113245, 20.00000000000000000 ) ) ;
#3896 = DIRECTION ( 'NONE',  ( 0.9496839325805427334, 0.3132098788326367345, 0.000000000000000000 ) ) ;
#3897 = ORIENTED_EDGE ( 'NONE', *, *, #13123, .T. ) ;
#3898 = CARTESIAN_POINT ( 'NONE',  ( -18.05918829504999934, 10.97290950744599947, 60.04999999999999716 ) ) ;
#3899 = DIRECTION ( 'NONE',  ( 0.000000000000000000, 0.000000000000000000, 1.000000000000000000 ) ) ;
#3900 = DIRECTION ( 'NONE',  ( 0.000000000000000000, 0.000000000000000000, -1.000000000000000000 ) ) ;
#3901 = CARTESIAN_POINT ( 'NONE',  ( 1.940811704950001770, 10.97290950744599947, 10.00000000000000000 ) ) ;
#3902 =( BOUNDED_CURVE ( )  B_SPLINE_CURVE ( 3, ( #2484, #4419, #12031, #7675 ),
 .UNSPECIFIED., .F., .T. ) 
 B_SPLINE_CURVE_WITH_KNOTS ( ( 4, 4 ),
 ( 0.000000000000000000, 1.570796326794890119 ),
 .UNSPECIFIED. ) 
 CURVE ( )  GEOMETRIC_REPRESENTATION_ITEM ( )  RATIONAL_B_SPLINE_CURVE ( ( 1.000000000000000000, 0.8047378541243663808, 0.8047378541243663808, 1.000000000000000000 ) ) 
 REPRESENTATION_ITEM ( '' )  );
#3903 = CARTESIAN_POINT ( 'NONE',  ( -36.21615338608749823, 23.36596564213564875, 68.85549045786049760 ) ) ;
#3904 = CARTESIAN_POINT ( 'NONE',  ( 44.88563590245420443, 0.000000000000000000, 23.00000000000000000 ) ) ;
#3905 = DIRECTION ( 'NONE',  ( 0.000000000000000000, 0.000000000000000000, 1.000000000000000000 ) ) ;
#3906 = CARTESIAN_POINT ( 'NONE',  ( 5.999999999999999112, 11.99999999999999822, 7.000000000000000000 ) ) ;
#3907 = CARTESIAN_POINT ( 'NONE',  ( -18.05918829504999934, 10.97290950744599947, 64.85000000000000853 ) ) ;
#3908 = UNCERTAINTY_MEASURE_WITH_UNIT (LENGTH_MEASURE( 1.000000000000000082E-05 ), #4660, 'distance_accuracy_value', 'NONE');
#3909 = ORIENTED_EDGE ( 'NONE', *, *, #7266, .T. ) ;
#3910 = EDGE_CURVE ( 'NONE', #11645, #7929, #9838, .T. ) ;
#3911 = ORIENTED_EDGE ( 'NONE', *, *, #11943, .T. ) ;
#3912 = CARTESIAN_POINT ( 'NONE',  ( 44.63563590245420443, 94.90549801902425031, 20.00000000000000000 ) ) ;
#3913 = EDGE_LOOP ( 'NONE', ( #5388, #11661, #2510, #522 ) ) ;
#3914 = ORIENTED_EDGE ( 'NONE', *, *, #3213, .F. ) ;
#3915 = DIRECTION ( 'NONE',  ( 0.000000000000000000, 0.000000000000000000, 1.000000000000000000 ) ) ;
#3916 = DIRECTION ( 'NONE',  ( -1.000000000000000000, 0.000000000000000000, 0.000000000000000000 ) ) ;
#3917 = DIRECTION ( 'NONE',  ( -0.9496839325805416232, -0.3132098788326400096, 0.000000000000000000 ) ) ;
#3918 = ADVANCED_FACE ( 'NONE', ( #5001 ), #11610, .F. ) ;
#3919 = AXIS2_PLACEMENT_3D ( 'NONE', #10082, #697, #3859 ) ;
#3920 = CARTESIAN_POINT ( 'NONE',  ( 44.63563590245421864, 85.03908161011133870, 19.25000000000000000 ) ) ;
#3921 = FACE_OUTER_BOUND ( 'NONE', #9301, .T. ) ;
#3922 = FACE_OUTER_BOUND ( 'NONE', #9427, .T. ) ;
#3923 = VERTEX_POINT ( 'NONE', #12479 ) ;
#3924 = ADVANCED_FACE ( 'NONE', ( #9053 ), #11153, .T. ) ;
#3925 = CIRCLE ( 'NONE', #13061, 4.750000000000000888 ) ;
#3926 = ORIENTED_EDGE ( 'NONE', *, *, #9962, .T. ) ;
#3927 = CARTESIAN_POINT ( 'NONE',  ( -15.26929014322137945, 30.19213140065401646, 60.32611073319715445 ) ) ;
#3928 = EDGE_LOOP ( 'NONE', ( #12987, #6253, #2618, #4889 ) ) ;
#3929 = ORIENTED_EDGE ( 'NONE', *, *, #6306, .F. ) ;
#3930 = CARTESIAN_POINT ( 'NONE',  ( 100.2760581142613603, 115.9375248198690826, 10.00000000000000000 ) ) ;
#3931 = DIRECTION ( 'NONE',  ( 0.000000000000000000, 0.000000000000000000, -1.000000000000000000 ) ) ;
#3932 = ORIENTED_EDGE ( 'NONE', *, *, #13287, .T. ) ;
#3933 = CARTESIAN_POINT ( 'NONE',  ( -18.05918829504999934, 7.130333642789880244, 17.25000000000000000 ) ) ;
#3934 = DIRECTION ( 'NONE',  ( -1.000000000000000000, 0.000000000000000000, 0.000000000000000000 ) ) ;
#3935 = EDGE_CURVE ( 'NONE', #10398, #11868, #6888, .T. ) ;
#3936 = LINE ( 'NONE', #12327, #10725 ) ;
#3937 = DIRECTION ( 'NONE',  ( 0.000000000000000000, 0.000000000000000000, 1.000000000000000000 ) ) ;
#3938 = DIRECTION ( 'NONE',  ( 0.4528443260392607250, 0.8915896008669278450, 0.000000000000000000 ) ) ;
#3939 = CIRCLE ( 'NONE', #6137, 6.000000000000005329 ) ;
#3940 = LINE ( 'NONE', #520, #11838 ) ;
#3941 = VERTEX_POINT ( 'NONE', #1084 ) ;
#3942 = ORIENTED_EDGE ( 'NONE', *, *, #5729, .T. ) ;
#3943 = AXIS2_PLACEMENT_3D ( 'NONE', #12017, #9866, #9713 ) ;
#3944 = ORIENTED_EDGE ( 'NONE', *, *, #8975, .T. ) ;
#3945 = ORIENTED_EDGE ( 'NONE', *, *, #847, .F. ) ;
#3946 = ORIENTED_EDGE ( 'NONE', *, *, #12646, .T. ) ;
#3947 = FACE_OUTER_BOUND ( 'NONE', #6566, .T. ) ;
#3948 = EDGE_CURVE ( 'NONE', #6401, #1534, #10955, .T. ) ;
#3949 = CARTESIAN_POINT ( 'NONE',  ( -32.05918829504999934, -6.027090492554000534, 10.00000000000000000 ) ) ;
#3950 = DIRECTION ( 'NONE',  ( 0.000000000000000000, 0.000000000000000000, 1.000000000000000000 ) ) ;
#3951 = CARTESIAN_POINT ( 'NONE',  ( 3.940811704950009542, -14.02709049255400053, 0.000000000000000000 ) ) ;
#3952 = DIRECTION ( 'NONE',  ( -0.000000000000000000, -0.000000000000000000, -1.000000000000000000 ) ) ;
#3953 = FACE_OUTER_BOUND ( 'NONE', #4511, .T. ) ;
#3954 = APPLICATION_PROTOCOL_DEFINITION ( 'draft international standard', 'automotive_design', 1998, #5447 ) ;
#3955 = ORIENTED_EDGE ( 'NONE', *, *, #1329, .T. ) ;
#3956 = ORIENTED_EDGE ( 'NONE', *, *, #3856, .F. ) ;
#3957 = FACE_OUTER_BOUND ( 'NONE', #2229, .T. ) ;
#3958 = CARTESIAN_POINT ( 'NONE',  ( -16.07440008066354764, 8.723328269963658954, 24.10000000000000142 ) ) ;
#3959 = ORIENTED_EDGE ( 'NONE', *, *, #5440, .T. ) ;
#3960 = DIRECTION ( 'NONE',  ( 0.000000000000000000, 0.000000000000000000, 1.000000000000000000 ) ) ;
#3961 = LINE ( 'NONE', #8355, #147 ) ;
#3962 = DIRECTION ( 'NONE',  ( 0.000000000000000000, 1.000000000000000000, -0.000000000000000000 ) ) ;
#3963 = CARTESIAN_POINT ( 'NONE',  ( -18.05918829504999934, 10.97290950744599947, 5.250000000000000000 ) ) ;
#3964 = CARTESIAN_POINT ( 'NONE',  ( 134.6356359024541973, 89.90549801902423610, 22.89644660940672694 ) ) ;
#3965 = DIRECTION ( 'NONE',  ( -1.000000000000000000, -2.649577643422789356E-15, 0.000000000000000000 ) ) ;
#3966 = DIRECTION ( 'NONE',  ( -1.000000000000000000, 0.000000000000000000, 0.000000000000000000 ) ) ;
#3967 = CARTESIAN_POINT ( 'NONE',  ( -27.49999999999998934, 9.000000000000000000, -30.00000000000000355 ) ) ;
#3968 = FACE_BOUND ( 'NONE', #13406, .T. ) ;
#3969 = EDGE_CURVE ( 'NONE', #7909, #5579, #1576, .T. ) ;
#3970 = EDGE_CURVE ( 'NONE', #8162, #3627, #2153, .T. ) ;
#3971 = AXIS2_PLACEMENT_3D ( 'NONE', #8030, #2758, #11257 ) ;
#3972 = VECTOR ( 'NONE', #12741, 1000.000000000000000 ) ;
#3973 = EDGE_CURVE ( 'NONE', #11479, #12033, #3371, .T. ) ;
#3974 = COLOUR_RGB ( '', 0.09019608, 0.27058824, 0.51372549) ;
#3975 = ORIENTED_EDGE ( 'NONE', *, *, #10464, .T. ) ;
#3976 = VERTEX_POINT ( 'NONE', #40 ) ;
#3977 = DIRECTION ( 'NONE',  ( 1.000000000000000000, 8.673617379884027583E-16, -0.000000000000000000 ) ) ;
#3978 = ORIENTED_EDGE ( 'NONE', *, *, #2016, .F. ) ;
#3979 = VERTEX_POINT ( 'NONE', #8488 ) ;
#3980 = VERTEX_POINT ( 'NONE', #6175 ) ;
#3981 = CARTESIAN_POINT ( 'NONE',  ( -20.45469220996243820, -1.832421873814833901, 7.000000000000000000 ) ) ;
#3982 = DIRECTION ( 'NONE',  ( 0.000000000000000000, 0.000000000000000000, 1.000000000000000000 ) ) ;
#3983 = VECTOR ( 'NONE', #9644, 1000.000000000000000 ) ;
#3984 = AXIS2_PLACEMENT_3D ( 'NONE', #10417, #6220, #845 ) ;
#3985 = VECTOR ( 'NONE', #13317, 1000.000000000000000 ) ;
#3986 = DIRECTION ( 'NONE',  ( 0.000000000000000000, -1.000000000000000000, 0.000000000000000000 ) ) ;
#3987 = VECTOR ( 'NONE', #13501, 1000.000000000000114 ) ;
#3988 = DIRECTION ( 'NONE',  ( 0.000000000000000000, 0.000000000000000000, -1.000000000000000000 ) ) ;
#3989 = CARTESIAN_POINT ( 'NONE',  ( -18.05918829504999934, 14.81548537210212046, 68.85549045786049760 ) ) ;
#3990 = EDGE_CURVE ( 'NONE', #11751, #13530, #12934, .T. ) ;
#3991 = EDGE_CURVE ( 'NONE', #9550, #12241, #957, .T. ) ;
#3992 = ADVANCED_FACE ( 'NONE', ( #6463 ), #4313, .T. ) ;
#3993 = AXIS2_PLACEMENT_3D ( 'NONE', #12790, #2190, #1113 ) ;
#3994 = CIRCLE ( 'NONE', #7098, 7.833333332999988130 ) ;
#3995 = ORIENTED_EDGE ( 'NONE', *, *, #11318, .T. ) ;
#3996 = AXIS2_PLACEMENT_3D ( 'NONE', #9378, #5934, #7970 ) ;
#3997 = EDGE_CURVE ( 'NONE', #6107, #9550, #9541, .T. ) ;
#3998 = VERTEX_POINT ( 'NONE', #10589 ) ;
#3999 = CARTESIAN_POINT ( 'NONE',  ( -15.09142106175067788, 30.16999431241942276, 54.60426940283544184 ) ) ;
#4000 = ORIENTED_EDGE ( 'NONE', *, *, #13629, .F. ) ;
#4001 = ORIENTED_EDGE ( 'NONE', *, *, #12876, .T. ) ;
#4002 = CARTESIAN_POINT ( 'NONE',  ( 141.8856359024541973, 99.03908161011133870, 0.000000000000000000 ) ) ;
#4003 = SURFACE_SIDE_STYLE ('',( #3176 ) ) ;
#4004 = LINE ( 'NONE', #6142, #7589 ) ;
#4005 = CARTESIAN_POINT ( 'NONE',  ( -18.05918829504999934, 10.97290950744599947, 62.85000000000000142 ) ) ;
#4006 = FACE_OUTER_BOUND ( 'NONE', #5851, .T. ) ;
#4007 = ORIENTED_EDGE ( 'NONE', *, *, #5747, .F. ) ;
#4008 = DIRECTION ( 'NONE',  ( 0.000000000000000000, 0.000000000000000000, -1.000000000000000000 ) ) ;
#4009 = DIRECTION ( 'NONE',  ( 0.000000000000000000, 0.000000000000000000, 1.000000000000000000 ) ) ;
#4010 = DIRECTION ( 'NONE',  ( -1.000000000000000000, 0.000000000000000000, 0.000000000000000000 ) ) ;
#4011 = EDGE_CURVE ( 'NONE', #12154, #13705, #9477, .T. ) ;
#4012 = LINE ( 'NONE', #13358, #6250 ) ;
#4013 = AXIS2_PLACEMENT_3D ( 'NONE', #4213, #4288, #8531 ) ;
#4014 = ADVANCED_FACE ( 'NONE', ( #6390 ), #3069, .F. ) ;
#4015 = ORIENTED_EDGE ( 'NONE', *, *, #2127, .T. ) ;
#4016 = ADVANCED_FACE ( 'NONE', ( #2224 ), #8554, .T. ) ;
#4017 = VERTEX_POINT ( 'NONE', #13663 ) ;
#4018 = ORIENTED_EDGE ( 'NONE', *, *, #8442, .T. ) ;
#4019 = EDGE_LOOP ( 'NONE', ( #4370, #13382 ) ) ;
#4020 = AXIS2_PLACEMENT_3D ( 'NONE', #1423, #10099, #8051 ) ;
#4021 = AXIS2_PLACEMENT_3D ( 'NONE', #176, #7428, #7364 ) ;
#4022 = ORIENTED_EDGE ( 'NONE', *, *, #9485, .T. ) ;
#4023 = LINE ( 'NONE', #12338, #7981 ) ;
#4024 = CARTESIAN_POINT ( 'NONE',  ( -20.36713024065852551, 30.24535125755222609, 60.82066359492309005 ) ) ;
#4025 = DIRECTION ( 'NONE',  ( 0.000000000000000000, 1.672022627447524993E-15, 1.000000000000000000 ) ) ;
#4026 = CARTESIAN_POINT ( 'NONE',  ( -4.284128961655960133, 3.976464670139415070, 60.65000000000000568 ) ) ;
#4027 = CYLINDRICAL_SURFACE ( 'NONE', #10527, 1.999999999999986233 ) ;
#4028 = ADVANCED_FACE ( 'NONE', ( #11646 ), #11572, .F. ) ;
#4029 = DIRECTION ( 'NONE',  ( 0.000000000000000000, 0.000000000000000000, -1.000000000000000000 ) ) ;
#4030 = DIRECTION ( 'NONE',  ( 1.224646799147353207E-16, 0.000000000000000000, -1.000000000000000000 ) ) ;
#4031 = CIRCLE ( 'NONE', #10940, 0.5000000000000004441 ) ;
#4032 = AXIS2_PLACEMENT_3D ( 'NONE', #13778, #3200, #7412 ) ;
#4033 = ADVANCED_FACE ( 'NONE', ( #4376 ), #12555, .T. ) ;
#4034 = CARTESIAN_POINT ( 'NONE',  ( -34.55918829505000645, 10.97290950744599947, 57.35000000000000142 ) ) ;
#4035 = CARTESIAN_POINT ( 'NONE',  ( 6.940811704950001548, 32.97290950744599769, 10.00000000000000000 ) ) ;
#4036 = ORIENTED_EDGE ( 'NONE', *, *, #10743, .T. ) ;
#4037 = DIRECTION ( 'NONE',  ( 0.000000000000000000, 0.000000000000000000, -1.000000000000000000 ) ) ;
#4038 = CARTESIAN_POINT ( 'NONE',  ( -34.72201093190195564, 10.97290950744599947, 17.25000000000000000 ) ) ;
#4039 = LINE ( 'NONE', #11648, #32 ) ;
#4040 = AXIS2_PLACEMENT_3D ( 'NONE', #10321, #13383, #1720 ) ;
#4041 = CIRCLE ( 'NONE', #8477, 6.000000000000002665 ) ;
#4042 = AXIS2_PLACEMENT_3D ( 'NONE', #13498, #3729, #7976 ) ;
#4043 = DIRECTION ( 'NONE',  ( 1.000000000000000000, 0.000000000000000000, 0.000000000000000000 ) ) ;
#4044 = DIRECTION ( 'NONE',  ( 0.000000000000000000, 0.000000000000000000, 1.000000000000000000 ) ) ;
#4045 = CONICAL_SURFACE ( 'NONE', #6251, 3.800000000000001155, 0.7853981633974476129 ) ;
#4046 = DIRECTION ( 'NONE',  ( 0.000000000000000000, 0.000000000000000000, -1.000000000000000000 ) ) ;
#4047 = CARTESIAN_POINT ( 'NONE',  ( -23.57208814848684852, -7.366404416634599883, 62.14999999999999858 ) ) ;
#4048 = CARTESIAN_POINT ( 'NONE',  ( -18.05918829504999934, 10.97290950744599947, 57.54999999999999716 ) ) ;
#4049 = PRESENTATION_STYLE_ASSIGNMENT (( #7170 ) ) ;
#4050 = PRODUCT_DEFINITION_CONTEXT ( 'detailed design', #8323, 'design' ) ;
#4051 = ORIENTED_EDGE ( 'NONE', *, *, #2178, .F. ) ;
#4052 = AXIS2_PLACEMENT_3D ( 'NONE', #5108, #2903, #13554 ) ;
#4053 = CONICAL_SURFACE ( 'NONE', #5142, 6.049999999999999822, 0.1357715569457985105 ) ;
#4054 = APPLICATION_CONTEXT ( 'automotive_design' ) ;
#4055 = ORIENTED_EDGE ( 'NONE', *, *, #1353, .F. ) ;
#4056 = CIRCLE ( 'NONE', #2729, 2.700000000000000178 ) ;
#4057 = ORIENTED_EDGE ( 'NONE', *, *, #892, .F. ) ;
#4058 = CARTESIAN_POINT ( 'NONE',  ( -5.789834139046009298, 27.54455229823479812, 7.250000000000000000 ) ) ;
#4059 = ORIENTED_EDGE ( 'NONE', *, *, #4182, .T. ) ;
#4060 = EDGE_CURVE ( 'NONE', #2748, #3674, #11398, .T. ) ;
#4061 = ORIENTED_EDGE ( 'NONE', *, *, #13177, .T. ) ;
#4062 = ORIENTED_EDGE ( 'NONE', *, *, #4182, .F. ) ;
#4063 = DIRECTION ( 'NONE',  ( 0.000000000000000000, 0.000000000000000000, -1.000000000000000000 ) ) ;
#4064 = DIRECTION ( 'NONE',  ( -0.6615960714621565986, 0.7498604124941128379, 0.000000000000000000 ) ) ;
#4065 = LINE ( 'NONE', #11315, #13411 ) ;
#4066 = DIRECTION ( 'NONE',  ( 1.000000000000000000, 0.000000000000000000, 0.000000000000000000 ) ) ;
#4067 = PRESENTATION_LAYER_ASSIGNMENT (  '', '', ( #9412 ) ) ;
#4068 = CIRCLE ( 'NONE', #9406, 4.750000000000000000 ) ;
#4069 = LINE ( 'NONE', #12578, #13771 ) ;
#4070 = CIRCLE ( 'NONE', #5594, 18.50000000000000000 ) ;
#4071 = VERTEX_POINT ( 'NONE', #4109 ) ;
#4072 =( GEOMETRIC_REPRESENTATION_CONTEXT ( 3 ) GLOBAL_UNCERTAINTY_ASSIGNED_CONTEXT ( ( #10614 ) ) GLOBAL_UNIT_ASSIGNED_CONTEXT ( ( #5489, #9807, #11787 ) ) REPRESENTATION_CONTEXT ( 'NONE', 'WORKASPACE' ) );
#4073 = CARTESIAN_POINT ( 'NONE',  ( -14.22962324644737286, 30.04243591129733559, 57.08230891415405495 ) ) ;
#4074 = ORIENTED_EDGE ( 'NONE', *, *, #1770, .T. ) ;
#4075 = EDGE_CURVE ( 'NONE', #7400, #5675, #3137, .T. ) ;
#4076 = ORIENTED_EDGE ( 'NONE', *, *, #7438, .T. ) ;
#4077 = DIRECTION ( 'NONE',  ( 0.000000000000000000, 0.000000000000000000, 1.000000000000000000 ) ) ;
#4078 = DIRECTION ( 'NONE',  ( 0.000000000000000000, 0.000000000000000000, -1.000000000000000000 ) ) ;
#4079 = VERTEX_POINT ( 'NONE', #2088 ) ;
#4080 = CARTESIAN_POINT ( 'NONE',  ( -12.00000000000000000, 2.500000000000000000, -65.00000000000000000 ) ) ;
#4081 = CARTESIAN_POINT ( 'NONE',  ( -19.71317847370539766, 12.84756053868127879, 67.84999999999999432 ) ) ;
#4082 = ORIENTED_EDGE ( 'NONE', *, *, #13544, .F. ) ;
#4083 = DIRECTION ( 'NONE',  ( 0.000000000000000000, 0.000000000000000000, 1.000000000000000000 ) ) ;
#4084 = DIRECTION ( 'NONE',  ( 0.000000000000000000, 0.000000000000000000, -1.000000000000000000 ) ) ;
#4085 = DIRECTION ( 'NONE',  ( 1.000000000000000000, 1.387778780781446464E-15, 0.000000000000000000 ) ) ;
#4086 = CYLINDRICAL_SURFACE ( 'NONE', #6925, 34.70000000000000284 ) ;
#4087 = ADVANCED_FACE ( 'NONE', ( #513, #2769, #13281, #1689, #6594, #574, #9026, #1554 ), #3721, .T. ) ;
#4088 = ORIENTED_EDGE ( 'NONE', *, *, #6277, .T. ) ;
#4089 = ORIENTED_EDGE ( 'NONE', *, *, #8957, .T. ) ;
#4090 = EDGE_CURVE ( 'NONE', #10605, #2697, #13179, .T. ) ;
#4091 = ORIENTED_EDGE ( 'NONE', *, *, #1329, .F. ) ;
#4092 = AXIS2_PLACEMENT_3D ( 'NONE', #8275, #2787, #6096 ) ;
#4093 = EDGE_LOOP ( 'NONE', ( #8233, #287, #862, #6235 ) ) ;
#4094 = CARTESIAN_POINT ( 'NONE',  ( -18.05918829504999934, 10.97290950744599947, 63.35000000000000142 ) ) ;
#4095 = CARTESIAN_POINT ( 'NONE',  ( -18.87229898793585292, 30.34604302011655363, 61.60856125853900522 ) ) ;
#4096 = CARTESIAN_POINT ( 'NONE',  ( 50.63563590245420443, 108.9054980190242503, 23.00000000000000000 ) ) ;
#4097 = CARTESIAN_POINT ( 'NONE',  ( -18.05918829504999934, 10.97290950744599947, 60.04999999999999716 ) ) ;
#4098 = CARTESIAN_POINT ( 'NONE',  ( 92.63563590245421153, 99.03908161011133870, 0.7500000000000006661 ) ) ;
#4099 = EDGE_CURVE ( 'NONE', #2443, #4079, #8953, .T. ) ;
#4100 = LINE ( 'NONE', #8347, #1104 ) ;
#4101 = PRODUCT_CONTEXT ( 'NONE', #9568, 'mechanical' ) ;
#4102 = ORIENTED_EDGE ( 'NONE', *, *, #8509, .F. ) ;
#4103 = ORIENTED_EDGE ( 'NONE', *, *, #126, .F. ) ;
#4104 = AXIS2_PLACEMENT_3D ( 'NONE', #5880, #10159, #4841 ) ;
#4105 = ADVANCED_FACE ( 'NONE', ( #5803 ), #6990, .T. ) ;
#4106 = DIRECTION ( 'NONE',  ( 0.000000000000000000, 1.000000000000000000, 0.000000000000000000 ) ) ;
#4107 = ORIENTED_EDGE ( 'NONE', *, *, #13109, .T. ) ;
#4108 = ORIENTED_EDGE ( 'NONE', *, *, #2585, .T. ) ;
#4109 = CARTESIAN_POINT ( 'NONE',  ( 50.63563590245420443, 94.90549801902425031, 20.00000000000000000 ) ) ;
#4110 = CARTESIAN_POINT ( 'NONE',  ( 50.63563590245420443, 103.9054980190242361, 23.00000000000000000 ) ) ;
#4111 = AXIS2_PLACEMENT_3D ( 'NONE', #7501, #12006, #9985 ) ;
#4112 = CARTESIAN_POINT ( 'NONE',  ( -18.05918829504999934, 10.97290950744599947, 27.09999999999999787 ) ) ;
#4113 = CARTESIAN_POINT ( 'NONE',  ( -18.05918829504999934, 10.97290950744599947, 61.65955166399999854 ) ) ;
#4114 = VERTEX_POINT ( 'NONE', #6926 ) ;
#4115 = CARTESIAN_POINT ( 'NONE',  ( 116.7775623211734342, 123.0390816101113245, 0.7500000000000006661 ) ) ;
#4116 = DIRECTION ( 'NONE',  ( 0.000000000000000000, 0.000000000000000000, -1.000000000000000000 ) ) ;
#4117 = LINE ( 'NONE', #5273, #1586 ) ;
#4118 = EDGE_CURVE ( 'NONE', #2746, #3005, #8491, .T. ) ;
#4119 = DIRECTION ( 'NONE',  ( 1.000000000000000000, 0.000000000000000000, 0.000000000000000000 ) ) ;
#4120 = ORIENTED_EDGE ( 'NONE', *, *, #6239, .F. ) ;
#4121 = ORIENTED_EDGE ( 'NONE', *, *, #6752, .F. ) ;
#4122 = ORIENTED_EDGE ( 'NONE', *, *, #6634, .T. ) ;
#4123 = DIRECTION ( 'NONE',  ( 0.000000000000000000, 0.000000000000000000, 1.000000000000000000 ) ) ;
#4124 = ORIENTED_EDGE ( 'NONE', *, *, #730, .F. ) ;
#4125 = ORIENTED_EDGE ( 'NONE', *, *, #669, .T. ) ;
#4126 = CARTESIAN_POINT ( 'NONE',  ( -20.10273234482015425, 15.83781399370707810, 68.57331103393035221 ) ) ;
#4127 = LINE ( 'NONE', #3085, #5364 ) ;
#4128 = CARTESIAN_POINT ( 'NONE',  ( 134.8856359024541973, 108.6554980190242503, 23.00000000000000000 ) ) ;
#4129 = DIRECTION ( 'NONE',  ( 0.000000000000000000, 0.000000000000000000, -1.000000000000000000 ) ) ;
#4130 = ADVANCED_FACE ( 'NONE', ( #4775 ), #252, .F. ) ;
#4131 = ORIENTED_EDGE ( 'NONE', *, *, #2124, .F. ) ;
#4132 = CARTESIAN_POINT ( 'NONE',  ( -15.27375731803826397, 30.19267137862248163, 60.33151965850841236 ) ) ;
#4133 = ORIENTED_EDGE ( 'NONE', *, *, #13123, .F. ) ;
#4134 = ORIENTED_EDGE ( 'NONE', *, *, #10568, .F. ) ;
#4135 = CARTESIAN_POINT ( 'NONE',  ( -18.05918829504999934, 3.354823934416959919, 61.65955166408550525 ) ) ;
#4136 = CIRCLE ( 'NONE', #12391, 4.000000000000000888 ) ;
#4137 = LINE ( 'NONE', #3237, #2792 ) ;
#4138 = CARTESIAN_POINT ( 'NONE',  ( -20.37477454516755060, 13.59742095117539940, 68.84999999999999432 ) ) ;
#4139 = EDGE_LOOP ( 'NONE', ( #3239, #1181, #8565 ) ) ;
#4140 = DIRECTION ( 'NONE',  ( 1.182766006347823109E-16, -1.000000000000000000, 0.000000000000000000 ) ) ;
#4141 = CARTESIAN_POINT ( 'NONE',  ( -35.05918829505000645, 27.97290950744599769, 17.25000000000000000 ) ) ;
#4142 = FACE_OUTER_BOUND ( 'NONE', #4149, .T. ) ;
#4143 = DIRECTION ( 'NONE',  ( 0.4528443260392608916, 0.8915896008669277339, 0.000000000000000000 ) ) ;
#4144 = DIRECTION ( 'NONE',  ( 0.000000000000000000, 0.000000000000000000, -1.000000000000000000 ) ) ;
#4145 = EDGE_CURVE ( 'NONE', #6343, #2296, #914, .T. ) ;
#4146 = ADVANCED_FACE ( 'NONE', ( #11916 ), #13025, .T. ) ;
#4147 = ORIENTED_EDGE ( 'NONE', *, *, #8220, .F. ) ;
#4148 = ORIENTED_EDGE ( 'NONE', *, *, #5670, .F. ) ;
#4149 = EDGE_LOOP ( 'NONE', ( #9955, #5235, #5665, #2283 ) ) ;
#4150 = VERTEX_POINT ( 'NONE', #11266 ) ;
#4151 = ORIENTED_EDGE ( 'NONE', *, *, #13482, .T. ) ;
#4152 = DIRECTION ( 'NONE',  ( 0.000000000000000000, 0.000000000000000000, 1.000000000000000000 ) ) ;
#4153 = DIRECTION ( 'NONE',  ( 1.000000000000000000, 0.000000000000000000, 0.000000000000000000 ) ) ;
#4154 = ORIENTED_EDGE ( 'NONE', *, *, #3008, .F. ) ;
#4155 = VECTOR ( 'NONE', #2587, 1000.000000000000114 ) ;
#4156 = LINE ( 'NONE', #6029, #6503 ) ;
#4157 = CARTESIAN_POINT ( 'NONE',  ( -18.78165555769320960, 26.95724247477075153, 56.02363196900555664 ) ) ;
#4158 = DIRECTION ( 'NONE',  ( -0.000000000000000000, -0.000000000000000000, 1.000000000000000000 ) ) ;
#4159 = DIRECTION ( 'NONE',  ( -0.000000000000000000, 1.000000000000000000, -0.000000000000000000 ) ) ;
#4160 = CARTESIAN_POINT ( 'NONE',  ( -1.059188295049996231, 27.97290950744599769, 7.250000000000000000 ) ) ;
#4161 = ITEM_DEFINED_TRANSFORMATION ( 'NONE', 'NONE', #6445,  #6434 ) ;
#4162 = EDGE_CURVE ( 'NONE', #6593, #1954, #2438, .T. ) ;
#4163 = EDGE_CURVE ( 'NONE', #10962, #13429, #2300, .T. ) ;
#4164 = CIRCLE ( 'NONE', #5262, 6.419999999999999929 ) ;
#4165 = EDGE_CURVE ( 'NONE', #1026, #8282, #11618, .T. ) ;
#4166 = ORIENTED_EDGE ( 'NONE', *, *, #10315, .F. ) ;
#4167 = ADVANCED_FACE ( 'NONE', ( #8043, #12323 ), #2698, .T. ) ;
#4168 = DIRECTION ( 'NONE',  ( -0.000000000000000000, -1.000000000000000000, -0.000000000000000000 ) ) ;
#4169 = CARTESIAN_POINT ( 'NONE',  ( -1.059188295049996231, 10.97290950744599947, 57.35000000000000142 ) ) ;
#4170 = VERTEX_POINT ( 'NONE', #4833 ) ;
#4171 = DIRECTION ( 'NONE',  ( 0.000000000000000000, 0.000000000000000000, -1.000000000000000000 ) ) ;
#4172 = DIRECTION ( 'NONE',  ( 0.7071067811865524577, 0.7071067811865425767, -0.000000000000000000 ) ) ;
#4173 = FACE_OUTER_BOUND ( 'NONE', #2116, .T. ) ;
#4174 = CARTESIAN_POINT ( 'NONE',  ( -11.91335496205000055, 10.97290950744599947, 61.10999999999999943 ) ) ;
#4175 = DIRECTION ( 'NONE',  ( -0.000000000000000000, 0.000000000000000000, -1.000000000000000000 ) ) ;
#4176 = CARTESIAN_POINT ( 'NONE',  ( 75.58559257550551536, 115.9888905337886769, 0.7500000000000006661 ) ) ;
#4177 = CARTESIAN_POINT ( 'NONE',  ( 76.11748380738829667, 115.4601262030644762, 19.25000000000000000 ) ) ;
#4178 = AXIS2_PLACEMENT_3D ( 'NONE', #10473, #9492, #9700 ) ;
#4179 = DIRECTION ( 'NONE',  ( 1.000000000000000000, 0.000000000000000000, -0.000000000000000000 ) ) ;
#4180 = EDGE_CURVE ( 'NONE', #11456, #1687, #10222, .T. ) ;
#4181 = ORIENTED_EDGE ( 'NONE', *, *, #7644, .F. ) ;
#4182 = EDGE_CURVE ( 'NONE', #1263, #10693, #10963, .T. ) ;
#4183 = CIRCLE ( 'NONE', #9750, 1.999999999999996669 ) ;
#4184 = AXIS2_PLACEMENT_3D ( 'NONE', #1800, #10322, #743 ) ;
#4185 = EDGE_CURVE ( 'NONE', #10997, #467, #9161, .T. ) ;
#4186 = CARTESIAN_POINT ( 'NONE',  ( 140.3856359024541973, 94.65549801902425031, 23.00000000000000000 ) ) ;
#4187 = ORIENTED_EDGE ( 'NONE', *, *, #4163, .T. ) ;
#4188 = EDGE_LOOP ( 'NONE', ( #7507, #12754, #7359, #1914 ) ) ;
#4189 = VERTEX_POINT ( 'NONE', #10291 ) ;
#4190 = CARTESIAN_POINT ( 'NONE',  ( -20.08917107840481009, 15.84977899470587559, 68.56751079857853881 ) ) ;
#4191 = ORIENTED_EDGE ( 'NONE', *, *, #12377, .T. ) ;
#4192 = DIRECTION ( 'NONE',  ( 0.000000000000000000, 0.000000000000000000, 1.000000000000000000 ) ) ;
#4193 = CARTESIAN_POINT ( 'NONE',  ( 84.99521369064696330, 82.14063840035363739, 20.00000000000000000 ) ) ;
#4194 = LINE ( 'NONE', #5490, #5300 ) ;
#4195 = CARTESIAN_POINT ( 'NONE',  ( 98.63563590245422574, 99.03908161011133870, -30.00000000000001776 ) ) ;
#4196 = AXIS2_PLACEMENT_3D ( 'NONE', #7994, #6032, #8071 ) ;
#4197 = VECTOR ( 'NONE', #10661, 1000.000000000000000 ) ;
#4198 = MECHANICAL_DESIGN_GEOMETRIC_PRESENTATION_REPRESENTATION (  '', ( #6415 ), #4640 ) ;
#4199 = ORIENTED_EDGE ( 'NONE', *, *, #13592, .F. ) ;
#4200 = EDGE_CURVE ( 'NONE', #10920, #1852, #705, .T. ) ;
#4201 = CARTESIAN_POINT ( 'NONE',  ( -14.79170389260510277, 30.12932847815346094, 55.08659537360541947 ) ) ;
#4202 = AXIS2_PLACEMENT_3D ( 'NONE', #5571, #9861, #3496 ) ;
#4203 = EDGE_LOOP ( 'NONE', ( #7036, #6742, #13782, #5248 ) ) ;
#4204 = CIRCLE ( 'NONE', #1507, 6.000000000000000888 ) ;
#4205 = EDGE_LOOP ( 'NONE', ( #12975, #706, #2582, #8461 ) ) ;
#4206 = FACE_OUTER_BOUND ( 'NONE', #7374, .T. ) ;
#4207 = CIRCLE ( 'NONE', #625, 6.449999999999997513 ) ;
#4208 = PLANE ( 'NONE',  #9279 ) ;
#4209 = CARTESIAN_POINT ( 'NONE',  ( 0.000000000000000000, 104.1554980190242361, 22.75000000000000000 ) ) ;
#4210 = DIRECTION ( 'NONE',  ( 0.000000000000000000, 0.000000000000000000, -1.000000000000000000 ) ) ;
#4211 = DIRECTION ( 'NONE',  ( 1.000000000000000000, 0.000000000000000000, 0.000000000000000000 ) ) ;
#4212 = DIRECTION ( 'NONE',  ( 0.000000000000000000, -1.000000000000000000, 0.000000000000000000 ) ) ;
#4213 = CARTESIAN_POINT ( 'NONE',  ( -1.059188295049996231, 27.97290950744599769, 64.85000000000000853 ) ) ;
#4214 =( GEOMETRIC_REPRESENTATION_CONTEXT ( 3 ) GLOBAL_UNCERTAINTY_ASSIGNED_CONTEXT ( ( #2253 ) ) GLOBAL_UNIT_ASSIGNED_CONTEXT ( ( #2308, #4454, #5276 ) ) REPRESENTATION_CONTEXT ( 'NONE', 'WORKASPACE' ) );
#4215 = CIRCLE ( 'NONE', #7765, 2.000000000000001776 ) ;
#4216 = CIRCLE ( 'NONE', #12018, 17.50000000000000355 ) ;
#4217 = VERTEX_POINT ( 'NONE', #8178 ) ;
#4218 = ORIENTED_EDGE ( 'NONE', *, *, #4853, .F. ) ;
#4219 = EDGE_LOOP ( 'NONE', ( #12685, #13327, #1233, #5622 ) ) ;
#4220 = ORIENTED_EDGE ( 'NONE', *, *, #5959, .T. ) ;
#4221 = ORIENTED_EDGE ( 'NONE', *, *, #10411, .F. ) ;
#4222 = EDGE_CURVE ( 'NONE', #10012, #12272, #2721, .T. ) ;
#4223 = AXIS2_PLACEMENT_3D ( 'NONE', #4380, #3274, #174 ) ;
#4224 = DIRECTION ( 'NONE',  ( 0.6615960714621574867, -0.7498604124941119498, 0.000000000000000000 ) ) ;
#4225 = EDGE_CURVE ( 'NONE', #11449, #7400, #5155, .T. ) ;
#4226 = DIRECTION ( 'NONE',  ( -0.000000000000000000, -1.000000000000000000, -0.000000000000000000 ) ) ;
#4227 = AXIS2_PLACEMENT_3D ( 'NONE', #6395, #8494, #12761 ) ;
#4228 = ORIENTED_EDGE ( 'NONE', *, *, #2124, .T. ) ;
#4229 = CYLINDRICAL_SURFACE ( 'NONE', #4493, 10.00000000000000178 ) ;
#4230 = CARTESIAN_POINT ( 'NONE',  ( 112.1804561881462945, 113.0390816101113387, 0.7500000000000006661 ) ) ;
#4231 = DIRECTION ( 'NONE',  ( 0.000000000000000000, 0.000000000000000000, 1.000000000000000000 ) ) ;
#4232 = CARTESIAN_POINT ( 'NONE',  ( -37.75918829505000218, -6.027090492554000534, 58.85000000000000142 ) ) ;
#4233 = CARTESIAN_POINT ( 'NONE',  ( 50.63563590245420443, 89.90549801902423610, 23.00000000000000000 ) ) ;
#4234 = AXIS2_PLACEMENT_3D ( 'NONE', #10740, #8704, #8628 ) ;
#4235 = ORIENTED_EDGE ( 'NONE', *, *, #9214, .T. ) ;
#4236 = DIRECTION ( 'NONE',  ( -0.9496839325805428444, -0.3132098788326364569, 0.000000000000000000 ) ) ;
#4237 = ORIENTED_EDGE ( 'NONE', *, *, #3935, .T. ) ;
#4238 = CARTESIAN_POINT ( 'NONE',  ( -18.05918829504999934, 28.64232754551664684, 55.84999999999999432 ) ) ;
#4239 = CARTESIAN_POINT ( 'NONE',  ( -12.00000000000000000, -2.500000000000000444, 0.000000000000000000 ) ) ;
#4240 = EDGE_CURVE ( 'NONE', #5520, #12460, #8390, .T. ) ;
#4241 =( NAMED_UNIT ( * ) SI_UNIT ( $, .STERADIAN. ) SOLID_ANGLE_UNIT ( ) );
#4242 = CARTESIAN_POINT ( 'NONE',  ( -19.55384571722024489, 30.31214524169468660, 53.34041679414971782 ) ) ;
#4243 = DIRECTION ( 'NONE',  ( 0.000000000000000000, 0.000000000000000000, -1.000000000000000000 ) ) ;
#4244 = CYLINDRICAL_SURFACE ( 'NONE', #4227, 6.450000000000001066 ) ;
#4245 = ADVANCED_FACE ( 'NONE', ( #1981 ), #8324, .F. ) ;
#4246 = DIRECTION ( 'NONE',  ( -0.000000000000000000, -0.000000000000000000, -1.000000000000000000 ) ) ;
#4247 = PLANE ( 'NONE',  #12737 ) ;
#4248 = EDGE_CURVE ( 'NONE', #2002, #7472, #10502, .T. ) ;
#4249 = DIRECTION ( 'NONE',  ( 0.7071067811865474617, 0.000000000000000000, 0.7071067811865474617 ) ) ;
#4250 = AXIS2_PLACEMENT_3D ( 'NONE', #5764, #8993, #474 ) ;
#4251 = PRODUCT_DEFINITION_SHAPE ( 'NONE', 'NONE',  #13808 ) ;
#4252 = SHAPE_REPRESENTATION_RELATIONSHIP ( 'NONE' , 'NONE' ,  #13195, #8750 ) ;
#4253 = AXIS2_PLACEMENT_3D ( 'NONE', #3605, #4637, #8900 ) ;
#4254 = EDGE_CURVE ( 'NONE', #3193, #1212, #4004, .T. ) ;
#4255 = EDGE_CURVE ( 'NONE', #8825, #12804, #10503, .T. ) ;
#4256 = ORIENTED_EDGE ( 'NONE', *, *, #1488, .T. ) ;
#4257 = ORIENTED_EDGE ( 'NONE', *, *, #9679, .T. ) ;
#4258 = CIRCLE ( 'NONE', #13615, 0.5000000000000004441 ) ;
#4259 = DIRECTION ( 'NONE',  ( 0.000000000000000000, 0.000000000000000000, -1.000000000000000000 ) ) ;
#4260 = CIRCLE ( 'NONE', #2939, 34.69999999999999574 ) ;
#4261 = AXIS2_PLACEMENT_3D ( 'NONE', #7045, #2761, #1680 ) ;
#4262 = VECTOR ( 'NONE', #7724, 1000.000000000000227 ) ;
#4263 = EDGE_LOOP ( 'NONE', ( #1856, #13471, #10481, #6404 ) ) ;
#4265 = ADVANCED_FACE ( 'NONE', ( #8118 ), #10415, .F. ) ;
#4264 = ORIENTED_EDGE ( 'NONE', *, *, #130, .F. ) ;
#4266 = CARTESIAN_POINT ( 'NONE',  ( -14.33236984630097588, 7.593145069921623858, 68.84999999999999432 ) ) ;
#4267 = CARTESIAN_POINT ( 'NONE',  ( -1.059188295049996231, -6.027090492554000534, 17.25000000000000000 ) ) ;
#4268 = DIRECTION ( 'NONE',  ( -0.000000000000000000, -0.000000000000000000, -1.000000000000000000 ) ) ;
#4269 = CARTESIAN_POINT ( 'NONE',  ( -17.23821357112329977, 5.029341513162310484, 67.84999999999999432 ) ) ;
#4270 = FACE_OUTER_BOUND ( 'NONE', #12951, .T. ) ;
#4271 = ADVANCED_FACE ( 'NONE', ( #10488 ), #917, .F. ) ;
#4272 = AXIS2_PLACEMENT_3D ( 'NONE', #9745, #9829, #11200 ) ;
#4273 = AXIS2_PLACEMENT_3D ( 'NONE', #10752, #8789, #2172 ) ;
#4274 = AXIS2_PLACEMENT_3D ( 'NONE', #10193, #7938, #7026 ) ;
#4275 = ORIENTED_EDGE ( 'NONE', *, *, #3146, .F. ) ;
#4276 = CARTESIAN_POINT ( 'NONE',  ( -15.51133711870873455, 30.22015921542349304, 54.10466577694464263 ) ) ;
#4277 = ORIENTED_EDGE ( 'NONE', *, *, #9228, .F. ) ;
#4278 = VERTEX_POINT ( 'NONE', #4138 ) ;
#4279 = EDGE_CURVE ( 'NONE', #3112, #6060, #6712, .T. ) ;
#4280 = DIRECTION ( 'NONE',  ( 1.000000000000000000, 0.000000000000000000, 0.000000000000000000 ) ) ;
#4281 = AXIS2_PLACEMENT_3D ( 'NONE', #4112, #12557, #807 ) ;
#4282 = FACE_OUTER_BOUND ( 'NONE', #13057, .T. ) ;
#4283 = AXIS2_PLACEMENT_3D ( 'NONE', #5257, #8611, #3258 ) ;
#4284 = CARTESIAN_POINT ( 'NONE',  ( 7.500000000000000000, -0.5000000000000017764, -65.00000000000000000 ) ) ;
#4285 = CARTESIAN_POINT ( 'NONE',  ( -30.48673169511680214, 10.97290950744599947, 83.57661607529820458 ) ) ;
#4286 = CARTESIAN_POINT ( 'NONE',  ( -24.37001676333060018, -4.028726038184999858, 62.14999999999999858 ) ) ;
#4287 = ADVANCED_FACE ( 'NONE', ( #12518 ), #11331, .T. ) ;
#4288 = DIRECTION ( 'NONE',  ( 0.000000000000000000, 0.000000000000000000, 1.000000000000000000 ) ) ;
#4289 = VECTOR ( 'NONE', #4600, 1000.000000000000000 ) ;
#4290 = ORIENTED_EDGE ( 'NONE', *, *, #3319, .F. ) ;
#4291 = VERTEX_POINT ( 'NONE', #1764 ) ;
#4292 = VERTEX_POINT ( 'NONE', #6300 ) ;
#4293 = ORIENTED_EDGE ( 'NONE', *, *, #8878, .F. ) ;
#4294 = CYLINDRICAL_SURFACE ( 'NONE', #5013, 6.145833333000002341 ) ;
#4295 = ORIENTED_EDGE ( 'NONE', *, *, #11747, .T. ) ;
#4296 = ORIENTED_EDGE ( 'NONE', *, *, #13427, .T. ) ;
#4297 = ORIENTED_EDGE ( 'NONE', *, *, #770, .T. ) ;
#4298 = CARTESIAN_POINT ( 'NONE',  ( 3.940811704950010430, -11.02709049255400053, 10.00000000000000000 ) ) ;
#4299 = DIRECTION ( 'NONE',  ( -1.000000000000000000, 0.000000000000000000, 0.000000000000000000 ) ) ;
#4300 = DIRECTION ( 'NONE',  ( 0.000000000000000000, 0.000000000000000000, 1.000000000000000000 ) ) ;
#4301 = AXIS2_PLACEMENT_3D ( 'NONE', #13028, #8910, #12053 ) ;
#4302 = DIRECTION ( 'NONE',  ( 0.000000000000000000, 0.000000000000000000, -1.000000000000000000 ) ) ;
#4303 = CARTESIAN_POINT ( 'NONE',  ( 84.99521369064696330, 82.14063840035363739, 10.00000000000000000 ) ) ;
#4304 = CARTESIAN_POINT ( 'NONE',  ( -36.21615338608749823, -1.420146627243662030, 7.250000000000000000 ) ) ;
#4305 = FACE_OUTER_BOUND ( 'NONE', #985, .T. ) ;
#4306 = PRODUCT_CONTEXT ( 'NONE', #12857, 'mechanical' ) ;
#4307 = VERTEX_POINT ( 'NONE', #10561 ) ;
#4308 = ADVANCED_FACE ( 'NONE', ( #4909 ), #9170, .T. ) ;
#4309 = AXIS2_PLACEMENT_3D ( 'NONE', #8132, #3887, #13504 ) ;
#4310 = ORIENTED_EDGE ( 'NONE', *, *, #5440, .F. ) ;
#4311 = CARTESIAN_POINT ( 'NONE',  ( -18.05918829504999934, 10.97290950744599947, 57.35000000000000142 ) ) ;
#4312 = DIRECTION ( 'NONE',  ( -0.7071067811865525687, -0.7071067811865425767, 0.000000000000000000 ) ) ;
#4313 = CYLINDRICAL_SURFACE ( 'NONE', #7814, 0.7500000000000006661 ) ;
#4314 = CARTESIAN_POINT ( 'NONE',  ( 72.18094369249178044, 97.20665973629650125, 10.00000000000000000 ) ) ;
#4315 = CARTESIAN_POINT ( 'NONE',  ( -18.79031867479901408, 30.34876749365192339, 53.07200068921699909 ) ) ;
#4317 = DIRECTION ( 'NONE',  ( -0.000000000000000000, -1.000000000000000000, -0.000000000000000000 ) ) ;
#4316 = APPLICATION_CONTEXT ( 'automotive_design' ) ;
#4318 = CARTESIAN_POINT ( 'NONE',  ( -38.38077571930825371, -0.4981161769137670281, 5.250000000000000000 ) ) ;
#4319 = DIRECTION ( 'NONE',  ( 0.000000000000000000, 0.000000000000000000, -1.000000000000000000 ) ) ;
#4320 = CARTESIAN_POINT ( 'NONE',  ( 140.6356359024541689, 85.03908161011133870, 19.25000000000000000 ) ) ;
#4321 = AXIS2_PLACEMENT_3D ( 'NONE', #13431, #11337, #1772 ) ;
#4322 = CYLINDRICAL_SURFACE ( 'NONE', #11375, 0.7499999999999973355 ) ;
#4323 =( NAMED_UNIT ( * ) PLANE_ANGLE_UNIT ( ) SI_UNIT ( $, .RADIAN. ) );
#4324 = EDGE_CURVE ( 'NONE', #6154, #8674, #241, .T. ) ;
#4325 = VERTEX_POINT ( 'NONE', #12916 ) ;
#4326 = CIRCLE ( 'NONE', #3662, 23.29163056034261459 ) ;
#4327 = DIRECTION ( 'NONE',  ( -1.000000000000000000, 0.000000000000000000, 0.000000000000000000 ) ) ;
#4328 = ORIENTED_EDGE ( 'NONE', *, *, #4987, .T. ) ;
#4329 = VERTEX_POINT ( 'NONE', #11805 ) ;
#4330 = ORIENTED_EDGE ( 'NONE', *, *, #10739, .T. ) ;
#4331 = CARTESIAN_POINT ( 'NONE',  ( -18.05918829504999934, 10.97290950744599947, 30.59999999999999787 ) ) ;
#4332 = PRODUCT_DEFINITION ( 'UNKNOWN', '', #13360, #9352 ) ;
#4333 = CARTESIAN_POINT ( 'NONE',  ( -3.759188295049999518, -6.027090492554000534, 7.250000000000000000 ) ) ;
#4334 = DIRECTION ( 'NONE',  ( 0.000000000000000000, 0.000000000000000000, -1.000000000000000000 ) ) ;
#4335 = DIRECTION ( 'NONE',  ( 0.000000000000000000, 0.000000000000000000, -1.000000000000000000 ) ) ;
#4336 = DIRECTION ( 'NONE',  ( 2.612535355386759959E-17, 0.000000000000000000, 1.000000000000000000 ) ) ;
#4337 = DIRECTION ( 'NONE',  ( -0.6615960714621565986, 0.7498604124941128379, 0.000000000000000000 ) ) ;
#4338 = ADVANCED_FACE ( 'NONE', ( #9508 ), #3294, .T. ) ;
#4339 = ORIENTED_EDGE ( 'NONE', *, *, #10147, .F. ) ;
#4340 = ADVANCED_FACE ( 'NONE', ( #10624 ), #8737, .T. ) ;
#4341 = AXIS2_PLACEMENT_3D ( 'NONE', #3930, #13090, #5874 ) ;
#4342 = LINE ( 'NONE', #7509, #1456 ) ;
#4343 = ORIENTED_EDGE ( 'NONE', *, *, #8576, .F. ) ;
#4344 = ORIENTED_EDGE ( 'NONE', *, *, #12872, .F. ) ;
#4345 =( NAMED_UNIT ( * ) SI_UNIT ( $, .STERADIAN. ) SOLID_ANGLE_UNIT ( ) );
#4346 = ADVANCED_FACE ( 'NONE', ( #4282 ), #3178, .T. ) ;
#4347 = DIRECTION ( 'NONE',  ( -0.7091883091770476710, -0.7050191076322684935, 0.000000000000000000 ) ) ;
#4348 = CARTESIAN_POINT ( 'NONE',  ( -34.05918829504999934, 10.97290950744599947, 64.85000000000000853 ) ) ;
#4349 = LINE ( 'NONE', #4284, #12699 ) ;
#4350 = FACE_OUTER_BOUND ( 'NONE', #1427, .T. ) ;
#4351 = CYLINDRICAL_SURFACE ( 'NONE', #10505, 23.22993838181875148 ) ;
#4352 = MANIFOLD_SOLID_BREP ( 'NONE', #5065 ) ;
#4353 = EDGE_CURVE ( 'NONE', #7731, #13005, #1185, .T. ) ;
#4354 = ORIENTED_EDGE ( 'NONE', *, *, #712, .F. ) ;
#4355 = ORIENTED_EDGE ( 'NONE', *, *, #9403, .T. ) ;
#4356 = CARTESIAN_POINT ( 'NONE',  ( -18.05918829504999934, 10.97290950744599947, 118.8499999999999943 ) ) ;
#4357 = VERTEX_POINT ( 'NONE', #8454 ) ;
#4358 = ORIENTED_EDGE ( 'NONE', *, *, #6716, .T. ) ;
#4359 = EDGE_LOOP ( 'NONE', ( #11012, #3344, #9662, #9926 ) ) ;
#4360 = ADVANCED_FACE ( 'NONE', ( #134 ), #5305, .F. ) ;
#4361 = ORIENTED_EDGE ( 'NONE', *, *, #7245, .T. ) ;
#4362 = DIRECTION ( 'NONE',  ( 0.000000000000000000, 0.000000000000000000, 1.000000000000000000 ) ) ;
#4363 = CARTESIAN_POINT ( 'NONE',  ( 42.63563590245419732, 85.78908161011133870, 0.7500000000000006661 ) ) ;
#4364 = VERTEX_POINT ( 'NONE', #9576 ) ;
#4365 = DIRECTION ( 'NONE',  ( 0.000000000000000000, 0.000000000000000000, -1.000000000000000000 ) ) ;
#4366 = CARTESIAN_POINT ( 'NONE',  ( -19.11830548702882737, 26.93836225865674194, 56.28610618890476047 ) ) ;
#4367 = CARTESIAN_POINT ( 'NONE',  ( -40.05918829505000645, 35.97290950744599058, 10.00000000000000000 ) ) ;
#4368 = DIRECTION ( 'NONE',  ( -0.000000000000000000, -0.000000000000000000, -1.000000000000000000 ) ) ;
#4369 = CARTESIAN_POINT ( 'NONE',  ( -9.759188295050000406, 10.97290950744599947, 61.86500000000000199 ) ) ;
#4370 = ORIENTED_EDGE ( 'NONE', *, *, #2519, .F. ) ;
#4371 = ORIENTED_EDGE ( 'NONE', *, *, #12206, .F. ) ;
#4372 = CIRCLE ( 'NONE', #123, 6.000000000000000888 ) ;
#4373 = EDGE_CURVE ( 'NONE', #3613, #7715, #5, .T. ) ;
#4374 = CARTESIAN_POINT ( 'NONE',  ( 0.000000000000000000, 4.500000000000000000, -23.49999999999999645 ) ) ;
#4375 = DIRECTION ( 'NONE',  ( 0.000000000000000000, 0.000000000000000000, -1.000000000000000000 ) ) ;
#4376 = FACE_OUTER_BOUND ( 'NONE', #5298, .T. ) ;
#4377 = CARTESIAN_POINT ( 'NONE',  ( -19.49808753468298406, 30.31569702816738854, 53.31359561727821017 ) ) ;
#4378 = DIRECTION ( 'NONE',  ( -1.000000000000000000, 0.000000000000000000, 0.000000000000000000 ) ) ;
#4379 = CARTESIAN_POINT ( 'NONE',  ( -2.842019651049983331, 18.58149382944601058, 61.98378871700000303 ) ) ;
#4380 = CARTESIAN_POINT ( 'NONE',  ( 81.82136590429890077, 114.1051029460540605, 20.00000000000000000 ) ) ;
#4381 = CARTESIAN_POINT ( 'NONE',  ( 4.000000000000001776, 2.000000000000000000, -65.00000000000000000 ) ) ;
#4382 = DIRECTION ( 'NONE',  ( 0.7071067811865451302, -0.7071067811865500152, 0.000000000000000000 ) ) ;
#4383 = AXIS2_PLACEMENT_3D ( 'NONE', #12186, #2639, #4578 ) ;
#4384 = ORIENTED_EDGE ( 'NONE', *, *, #6022, .F. ) ;
#4385 = DIRECTION ( 'NONE',  ( 0.000000000000000000, 0.000000000000000000, -1.000000000000000000 ) ) ;
#4386 = VERTEX_POINT ( 'NONE', #12724 ) ;
#4387 = ORIENTED_EDGE ( 'NONE', *, *, #2385, .T. ) ;
#4388 = VERTEX_POINT ( 'NONE', #7391 ) ;
#4389 = DIRECTION ( 'NONE',  ( 1.000000000000000000, 0.000000000000000000, 0.000000000000000000 ) ) ;
#4390 = CIRCLE ( 'NONE', #5486, 7.166108729582679970 ) ;
#4391 = DIRECTION ( 'NONE',  ( 1.000000000000000000, 0.000000000000000000, 0.000000000000000000 ) ) ;
#4392 = CARTESIAN_POINT ( 'NONE',  ( -16.04064420431702942, 0.000000000000000000, -9.307586582922249718 ) ) ;
#4393 = EDGE_CURVE ( 'NONE', #8669, #189, #10302, .T. ) ;
#4394 = CYLINDRICAL_SURFACE ( 'NONE', #12009, 0.7500000000000006661 ) ;
#4395 = EDGE_CURVE ( 'NONE', #8370, #665, #5505, .T. ) ;
#4396 = DIRECTION ( 'NONE',  ( 1.000000000000000000, 0.000000000000000000, 0.000000000000000000 ) ) ;
#4397 = FACE_OUTER_BOUND ( 'NONE', #5542, .T. ) ;
#4398 = CARTESIAN_POINT ( 'NONE',  ( 7.640422211807137209, 16.89844320975774750, 7.000000000000000000 ) ) ;
#4399 = EDGE_CURVE ( 'NONE', #13003, #13286, #8587, .T. ) ;
#4400 = EDGE_LOOP ( 'NONE', ( #6215, #12337 ) ) ;
#4401 = CARTESIAN_POINT ( 'NONE',  ( -16.49880428525771237, 30.30780693225702294, 53.37335251291963090 ) ) ;
#4402 = CARTESIAN_POINT ( 'NONE',  ( -18.05918829504999934, 10.97290950744599947, 5.250000000000000000 ) ) ;
#4403 = DIRECTION ( 'NONE',  ( 0.000000000000000000, 0.000000000000000000, 1.000000000000000000 ) ) ;
#4404 = FILL_AREA_STYLE_COLOUR ( '', #2290 ) ;
#4405 = DIRECTION ( 'NONE',  ( -0.9496839325805428444, -0.3132098788326364569, 0.000000000000000000 ) ) ;
#4406 = CARTESIAN_POINT ( 'NONE',  ( 0.000000000000000000, 0.000000000000000000, 0.000000000000000000 ) ) ;
#4407 = EDGE_CURVE ( 'NONE', #2401, #13684, #11633, .T. ) ;
#4408 = AXIS2_PLACEMENT_3D ( 'NONE', #2937, #7162, #11499 ) ;
#4409 = LINE ( 'NONE', #10699, #5553 ) ;
#4410 = FACE_BOUND ( 'NONE', #6869, .T. ) ;
#4411 = PRODUCT_DEFINITION_SHAPE ( 'NONE', 'NONE',  #12939 ) ;
#4412 = EDGE_CURVE ( 'NONE', #6343, #10722, #10696, .T. ) ;
#4413 = EDGE_CURVE ( 'NONE', #8730, #4170, #9072, .T. ) ;
#4414 = AXIS2_PLACEMENT_3D ( 'NONE', #6452, #29, #13773 ) ;
#4415 = VECTOR ( 'NONE', #5389, 1000.000000000000000 ) ;
#4416 = EDGE_LOOP ( 'NONE', ( #8535, #11635 ) ) ;
#4417 = ORIENTED_EDGE ( 'NONE', *, *, #369, .T. ) ;
#4418 = CIRCLE ( 'NONE', #13566, 1.500000000000001332 ) ;
#4419 = CARTESIAN_POINT ( 'NONE',  ( 142.6356359024541973, 111.0390816101113103, 19.68933982822018081 ) ) ;
#4420 = ORIENTED_EDGE ( 'NONE', *, *, #11486, .T. ) ;
#4421 = ORIENTED_EDGE ( 'NONE', *, *, #8106, .T. ) ;
#4422 =( BOUNDED_CURVE ( )  B_SPLINE_CURVE ( 3, ( #12671, #2076, #3255, #2284 ),
 .UNSPECIFIED., .F., .T. ) 
 B_SPLINE_CURVE_WITH_KNOTS ( ( 4, 4 ),
 ( 1.570796326794896558, 3.141592653589793116 ),
 .UNSPECIFIED. ) 
 CURVE ( )  GEOMETRIC_REPRESENTATION_ITEM ( )  RATIONAL_B_SPLINE_CURVE ( ( 1.000000000000000000, 0.8047378541243649375, 0.8047378541243649375, 1.000000000000000000 ) ) 
 REPRESENTATION_ITEM ( '' )  );
#4423 = DIRECTION ( 'NONE',  ( 0.000000000000000000, 0.000000000000000000, -1.000000000000000000 ) ) ;
#4424 = EDGE_CURVE ( 'NONE', #703, #2353, #12530, .T. ) ;
#4425 = LINE ( 'NONE', #9734, #8728 ) ;
#4426 = CIRCLE ( 'NONE', #6198, 6.049999999999999822 ) ;
#4427 = CARTESIAN_POINT ( 'NONE',  ( -17.56406670600707187, 26.96510319970443348, 55.93198005405052697 ) ) ;
#4428 = AXIS2_PLACEMENT_3D ( 'NONE', #10093, #5877, #9027 ) ;
#4429 = DIRECTION ( 'NONE',  ( -0.6615960714621569316, 0.7498604124941123938, 0.000000000000000000 ) ) ;
#4430 = AXIS2_PLACEMENT_3D ( 'NONE', #8722, #6350, #7500 ) ;
#4431 = CARTESIAN_POINT ( 'NONE',  ( -16.04064420431702942, 4.500000000000000000, -11.30758658292224084 ) ) ;
#4432 = AXIS2_PLACEMENT_3D ( 'NONE', #10058, #8932, #13389 ) ;
#4433 = ADVANCED_FACE ( 'NONE', ( #1401 ), #5581, .T. ) ;
#4434 = LINE ( 'NONE', #4717, #2038 ) ;
#4435 = APPLICATION_PROTOCOL_DEFINITION ( 'draft international standard', 'automotive_design', 1998, #6886 ) ;
#4436 = EDGE_CURVE ( 'NONE', #7400, #6357, #10981, .T. ) ;
#4437 = AXIS2_PLACEMENT_3D ( 'NONE', #12215, #6899, #7800 ) ;
#4438 = ORIENTED_EDGE ( 'NONE', *, *, #3815, .T. ) ;
#4439 = VECTOR ( 'NONE', #10838, 1000.000000000000000 ) ;
#4440 = AXIS2_PLACEMENT_3D ( 'NONE', #13727, #2028, #6266 ) ;
#4441 = EDGE_LOOP ( 'NONE', ( #2750, #8320 ) ) ;
#4442 = VECTOR ( 'NONE', #6146, 1000.000000000000000 ) ;
#4443 = DIRECTION ( 'NONE',  ( 0.3202092937642124215, 0.6304490528084107925, -0.7071067811865487940 ) ) ;
#4444 = CARTESIAN_POINT ( 'NONE',  ( -40.05918829504999934, -11.02709049255400053, 10.00000000000000000 ) ) ;
#4445 = CARTESIAN_POINT ( 'NONE',  ( -5.631644894983189431, 10.97290950744599947, 7.250000000000000000 ) ) ;
#4446 = DIRECTION ( 'NONE',  ( 1.000000000000000000, 0.000000000000000000, 0.000000000000000000 ) ) ;
#4447 = EDGE_CURVE ( 'NONE', #2636, #7944, #2610, .T. ) ;
#4448 = CYLINDRICAL_SURFACE ( 'NONE', #11634, 6.000000000000005329 ) ;
#4449 = ORIENTED_EDGE ( 'NONE', *, *, #6711, .F. ) ;
#4450 = CARTESIAN_POINT ( 'NONE',  ( -18.05918829504999934, 18.13068114044600065, 61.70038048199999281 ) ) ;
#4451 = DIRECTION ( 'NONE',  ( 0.000000000000000000, 0.000000000000000000, -1.000000000000000000 ) ) ;
#4452 = CARTESIAN_POINT ( 'NONE',  ( 140.3249757306743675, 85.78908161011133870, 20.00000000000000000 ) ) ;
#4453 = DIRECTION ( 'NONE',  ( 0.000000000000000000, 0.000000000000000000, -1.000000000000000000 ) ) ;
#4454 =( NAMED_UNIT ( * ) PLANE_ANGLE_UNIT ( ) SI_UNIT ( $, .RADIAN. ) );
#4455 = CONICAL_SURFACE ( 'NONE', #214, 16.95000000000000284, 0.7853981633974447263 ) ;
#4456 = EDGE_CURVE ( 'NONE', #8158, #11675, #13636, .T. ) ;
#4457 = VECTOR ( 'NONE', #11007, 1000.000000000000000 ) ;
#4458 = VERTEX_POINT ( 'NONE', #2681 ) ;
#4459 = CARTESIAN_POINT ( 'NONE',  ( 50.63563590245420443, 108.9054980190242503, 23.00000000000000000 ) ) ;
#4460 = ORIENTED_EDGE ( 'NONE', *, *, #2892, .T. ) ;
#4461 = ORIENTED_EDGE ( 'NONE', *, *, #2344, .F. ) ;
#4462 = CARTESIAN_POINT ( 'NONE',  ( 50.63563590245420443, 103.9054980190242361, 22.75000000000000000 ) ) ;
#4463 = PLANE ( 'NONE',  #5727 ) ;
#4464 = CARTESIAN_POINT ( 'NONE',  ( 116.7775623211734342, 85.78908161011133870, 19.25000000000000000 ) ) ;
#4465 = CIRCLE ( 'NONE', #13377, 0.9499999999999995115 ) ;
#4466 = AXIS2_PLACEMENT_3D ( 'NONE', #7921, #6751, #6601 ) ;
#4467 = DIRECTION ( 'NONE',  ( 0.000000000000000000, 0.000000000000000000, -1.000000000000000000 ) ) ;
#4468 = CARTESIAN_POINT ( 'NONE',  ( -30.30918829504999934, 27.97290950744599769, 68.85549045786049760 ) ) ;
#4469 = PLANE ( 'NONE',  #3434 ) ;
#4470 = LINE ( 'NONE', #7588, #1743 ) ;
#4471 = VECTOR ( 'NONE', #188, 1000.000000000000000 ) ;
#4472 = AXIS2_PLACEMENT_3D ( 'NONE', #9494, #12258, #6283 ) ;
#4473 = AXIS2_PLACEMENT_3D ( 'NONE', #9249, #9096, #10300 ) ;
#4474 = ORIENTED_EDGE ( 'NONE', *, *, #7926, .F. ) ;
#4475 = ADVANCED_FACE ( 'NONE', ( #12305, #12225 ), #10073, .T. ) ;
#4476 = CARTESIAN_POINT ( 'NONE',  ( -15.26283791438578419, 30.19135017472695637, 54.38173404877133521 ) ) ;
#4477 = ORIENTED_EDGE ( 'NONE', *, *, #5536, .F. ) ;
#4478 = DIRECTION ( 'NONE',  ( -0.000000000000000000, -0.000000000000000000, 1.000000000000000000 ) ) ;
#4479 = EDGE_LOOP ( 'NONE', ( #12259, #5174, #9103, #7571 ) ) ;
#4480 = DIRECTION ( 'NONE',  ( -0.000000000000000000, -0.000000000000000000, 1.000000000000000000 ) ) ;
#4481 = AXIS2_PLACEMENT_3D ( 'NONE', #5177, #13692, #7323 ) ;
#4482 = AXIS2_PLACEMENT_3D ( 'NONE', #4599, #12145, #540 ) ;
#4483 = CIRCLE ( 'NONE', #8940, 4.000000000000000888 ) ;
#4484 = CIRCLE ( 'NONE', #677, 2.700000000000001066 ) ;
#4485 = CYLINDRICAL_SURFACE ( 'NONE', #8682, 0.9499999999999995115 ) ;
#4486 = CARTESIAN_POINT ( 'NONE',  ( -38.38077571930825371, -0.4981161769137670281, 17.25000000000000000 ) ) ;
#4487 = MANIFOLD_SOLID_BREP ( 'Cut-Extrude1', #565 ) ;
#4488 = ORIENTED_EDGE ( 'NONE', *, *, #6099, .F. ) ;
#4489 = ADVANCED_FACE ( 'NONE', ( #4694 ), #9870, .T. ) ;
#4490 = VERTEX_POINT ( 'NONE', #7812 ) ;
#4491 = PRESENTATION_LAYER_ASSIGNMENT (  '', '', ( #6501 ) ) ;
#4492 = CARTESIAN_POINT ( 'NONE',  ( -1.059188295049996231, -6.027090492554000534, 7.250000000000000000 ) ) ;
#4493 = AXIS2_PLACEMENT_3D ( 'NONE', #1271, #12940, #7464 ) ;
#4494 = CIRCLE ( 'NONE', #12312, 5.999999999999997335 ) ;
#4495 = VERTEX_POINT ( 'NONE', #6776 ) ;
#4496 = VERTEX_POINT ( 'NONE', #291 ) ;
#4497 = ORIENTED_EDGE ( 'NONE', *, *, #1394, .T. ) ;
#4498 = LINE ( 'NONE', #6728, #1991 ) ;
#4499 = LINE ( 'NONE', #13010, #13777 ) ;
#4500 = ORIENTED_EDGE ( 'NONE', *, *, #75, .T. ) ;
#4501 = DIRECTION ( 'NONE',  ( -0.4528443260392611136, -0.8915896008669277339, 0.000000000000000000 ) ) ;
#4502 = CARTESIAN_POINT ( 'NONE',  ( -17.48907183174917890, 26.96265924644433198, 55.96010560725802918 ) ) ;
#4503 = DIRECTION ( 'NONE',  ( -1.000000000000000000, 0.000000000000000000, 0.000000000000000000 ) ) ;
#4504 = LINE ( 'NONE', #13016, #8961 ) ;
#4505 = DIRECTION ( 'NONE',  ( -0.000000000000000000, -0.000000000000000000, -1.000000000000000000 ) ) ;
#4506 = CIRCLE ( 'NONE', #8308, 1.999999999999991340 ) ;
#4507 = CIRCLE ( 'NONE', #12508, 1.999999999999991340 ) ;
#4508 = AXIS2_PLACEMENT_3D ( 'NONE', #6322, #12606, #8201 ) ;
#4509 = ORIENTED_EDGE ( 'NONE', *, *, #4436, .T. ) ;
#4510 = ADVANCED_FACE ( 'NONE', ( #4552 ), #13063, .T. ) ;
#4511 = EDGE_LOOP ( 'NONE', ( #12424, #5714, #5015, #5780 ) ) ;
#4512 = MANIFOLD_SOLID_BREP ( 'Cut-Extrude2', #9488 ) ;
#4513 = AXIS2_PLACEMENT_3D ( 'NONE', #5699, #12209, #7868 ) ;
#4514 = DIRECTION ( 'NONE',  ( 0.4528443260392610026, 0.8915896008669278450, 0.000000000000000000 ) ) ;
#4515 = CARTESIAN_POINT ( 'NONE',  ( -15.34212233881444831, 16.32244711264754855, 57.35000000000000142 ) ) ;
#4516 = CARTESIAN_POINT ( 'NONE',  ( -18.05918829504999934, 10.97290950744599947, 56.84999999999999432 ) ) ;
#4517 = DIRECTION ( 'NONE',  ( -1.000000000000000000, 0.000000000000000000, 0.000000000000000000 ) ) ;
#4518 = EDGE_CURVE ( 'NONE', #8191, #10863, #7823, .T. ) ;
#4519 = CARTESIAN_POINT ( 'NONE',  ( -19.81805515243290472, 30.29381900190004018, 53.48032518229263843 ) ) ;
#4520 =( NAMED_UNIT ( * ) PLANE_ANGLE_UNIT ( ) SI_UNIT ( $, .RADIAN. ) );
#4521 = EDGE_LOOP ( 'NONE', ( #12800, #9394, #11528, #2099 ) ) ;
#4522 = CARTESIAN_POINT ( 'NONE',  ( -18.05918829504999934, 3.352862570446000223, 61.63595870800000398 ) ) ;
#4523 = CARTESIAN_POINT ( 'NONE',  ( -18.05918829504999934, 10.97290950744599947, 61.86500000000000199 ) ) ;
#4524 = DIRECTION ( 'NONE',  ( -1.000000000000000000, 0.000000000000000000, 0.000000000000000000 ) ) ;
#4525 = CARTESIAN_POINT ( 'NONE',  ( 3.190811704950004657, -6.027090492554000534, 64.85000000000000853 ) ) ;
#4526 =( NAMED_UNIT ( * ) PLANE_ANGLE_UNIT ( ) SI_UNIT ( $, .RADIAN. ) );
#4527 = CIRCLE ( 'NONE', #11657, 1.999999999999995781 ) ;
#4528 = EDGE_CURVE ( 'NONE', #1552, #1301, #6944, .T. ) ;
#4529 = ORIENTED_EDGE ( 'NONE', *, *, #8063, .F. ) ;
#4530 = ORIENTED_EDGE ( 'NONE', *, *, #10067, .T. ) ;
#4531 = ORIENTED_EDGE ( 'NONE', *, *, #2343, .T. ) ;
#4532 = CARTESIAN_POINT ( 'NONE',  ( 3.940811704950009542, -14.02709049255400053, 10.00000000000000000 ) ) ;
#4533 = EDGE_LOOP ( 'NONE', ( #10333, #10689, #2538, #353 ) ) ;
#4534 = DIRECTION ( 'NONE',  ( -1.000000000000000000, 0.000000000000000000, -0.000000000000000000 ) ) ;
#4535 = DIRECTION ( 'NONE',  ( 1.000000000000000000, 0.000000000000000000, 0.000000000000000000 ) ) ;
#4536 = EDGE_CURVE ( 'NONE', #2, #12520, #12575, .T. ) ;
#4537 = FACE_OUTER_BOUND ( 'NONE', #9878, .T. ) ;
#4538 = CARTESIAN_POINT ( 'NONE',  ( -7.999999999999998224, 2.000000000000000000, 0.000000000000000000 ) ) ;
#4539 = CARTESIAN_POINT ( 'NONE',  ( -4.640588396653431147, -14.07073191448199978, 68.85549045786049760 ) ) ;
#4540 = ADVANCED_FACE ( 'NONE', ( #12501 ), #3395, .F. ) ;
#4541 = CARTESIAN_POINT ( 'NONE',  ( 16.08092853089229024, 4.500000000000000000, -9.237812082545193704 ) ) ;
#4542 = CARTESIAN_POINT ( 'NONE',  ( -5.309188295050000228, -6.027090492554000534, 64.35000000000000853 ) ) ;
#4543 = DIRECTION ( 'NONE',  ( 0.000000000000000000, -0.000000000000000000, 1.000000000000000000 ) ) ;
#4544 = CARTESIAN_POINT ( 'NONE',  ( -18.05918829504999934, 10.97290950744599947, 64.85000000000000853 ) ) ;
#4545 = TOROIDAL_SURFACE ( 'NONE', #9906, 10.75000000000000000, 0.7500000000000000000 ) ;
#4546 = EDGE_LOOP ( 'NONE', ( #10484, #13145 ) ) ;
#4547 = EDGE_LOOP ( 'NONE', ( #13328, #5944, #6642, #6790 ) ) ;
#4548 = CARTESIAN_POINT ( 'NONE',  ( -17.15591940245453273, 30.34273348207011622, 53.11510484006901578 ) ) ;
#4549 = ORIENTED_EDGE ( 'NONE', *, *, #315, .T. ) ;
#4550 =( LENGTH_UNIT ( ) NAMED_UNIT ( * ) SI_UNIT ( .MILLI., .METRE. ) );
#4551 = FACE_OUTER_BOUND ( 'NONE', #6276, .T. ) ;
#4552 = FACE_OUTER_BOUND ( 'NONE', #9834, .T. ) ;
#4553 = CYLINDRICAL_SURFACE ( 'NONE', #1532, 1.999999999999996669 ) ;
#4554 = DIRECTION ( 'NONE',  ( -0.000000000000000000, 0.000000000000000000, -1.000000000000000000 ) ) ;
#4555 = EDGE_CURVE ( 'NONE', #1146, #3112, #3827, .T. ) ;
#4556 = CARTESIAN_POINT ( 'NONE',  ( -12.00000000000000000, -2.500000000000000444, -65.00000000000000000 ) ) ;
#4557 = ORIENTED_EDGE ( 'NONE', *, *, #11880, .T. ) ;
#4558 = EDGE_LOOP ( 'NONE', ( #7366, #11473, #7569, #12734 ) ) ;
#4559 = DIRECTION ( 'NONE',  ( 0.000000000000000000, 0.000000000000000000, 1.000000000000000000 ) ) ;
#4560 = ORIENTED_EDGE ( 'NONE', *, *, #7709, .T. ) ;
#4561 = ORIENTED_EDGE ( 'NONE', *, *, #6820, .T. ) ;
#4562 = VERTEX_POINT ( 'NONE', #3029 ) ;
#4563 = VERTEX_POINT ( 'NONE', #13478 ) ;
#4564 = CYLINDRICAL_SURFACE ( 'NONE', #1975, 1.999999999999991340 ) ;
#4565 = CARTESIAN_POINT ( 'NONE',  ( 3.190811704950004657, 27.97290950744599769, 64.35000000000000853 ) ) ;
#4566 = EDGE_LOOP ( 'NONE', ( #4076, #11754 ) ) ;
#4567 = CARTESIAN_POINT ( 'NONE',  ( -30.32854245105399826, -5.598733283342819611, 64.85000000000000853 ) ) ;
#4568 = DIRECTION ( 'NONE',  ( -0.000000000000000000, -0.000000000000000000, 1.000000000000000000 ) ) ;
#4569 = EDGE_CURVE ( 'NONE', #3894, #2730, #5371, .T. ) ;
#4570 = CARTESIAN_POINT ( 'NONE',  ( -27.49999999999998934, 9.000000000000000000, 29.99999999999999645 ) ) ;
#4571 = EDGE_CURVE ( 'NONE', #1567, #9992, #4065, .T. ) ;
#4572 = CYLINDRICAL_SURFACE ( 'NONE', #661, 18.50000000000000000 ) ;
#4573 = ADVANCED_FACE ( 'NONE', ( #622 ), #1963, .F. ) ;
#4574 =( REPRESENTATION_RELATIONSHIP ('NONE','NONE', #11848, #11399 ) REPRESENTATION_RELATIONSHIP_WITH_TRANSFORMATION ( #12752 )SHAPE_REPRESENTATION_RELATIONSHIP( ) );
#4575 = ORIENTED_EDGE ( 'NONE', *, *, #10812, .T. ) ;
#4576 = ORIENTED_EDGE ( 'NONE', *, *, #6896, .T. ) ;
#4577 = MANIFOLD_SOLID_BREP ( 'Boss-Extrude1', #5904 ) ;
#4578 = DIRECTION ( 'NONE',  ( 0.4528443260392608916, 0.8915896008669277339, 0.000000000000000000 ) ) ;
#4579 = VECTOR ( 'NONE', #5724, 1000.000000000000000 ) ;
#4580 = CARTESIAN_POINT ( 'NONE',  ( -21.80975557129390907, 30.05623439618504023, 56.30605713593833173 ) ) ;
#4581 = DIRECTION ( 'NONE',  ( -0.7071067811865505703, 8.659560562354931626E-17, 0.7071067811865444641 ) ) ;
#4582 = DIRECTION ( 'NONE',  ( -1.000000000000000000, 0.000000000000000000, 0.000000000000000000 ) ) ;
#4583 = CARTESIAN_POINT ( 'NONE',  ( -30.32854245105399826, -5.598733283342819611, 68.85549045786049760 ) ) ;
#4584 = CARTESIAN_POINT ( 'NONE',  ( -18.05918829504999579, 18.25739707232493103, 61.99499741802014796 ) ) ;
#4585 = ADVANCED_FACE ( 'NONE', ( #10277 ), #690, .T. ) ;
#4586 = DIRECTION ( 'NONE',  ( -1.000000000000000000, 0.000000000000000000, 0.000000000000000000 ) ) ;
#4587 =( NAMED_UNIT ( * ) PLANE_ANGLE_UNIT ( ) SI_UNIT ( $, .RADIAN. ) );
#4588 = ORIENTED_EDGE ( 'NONE', *, *, #9233, .T. ) ;
#4589 = EDGE_CURVE ( 'NONE', #3872, #3046, #265, .T. ) ;
#4590 = EDGE_CURVE ( 'NONE', #3675, #12554, #8572, .T. ) ;
#4591 = VECTOR ( 'NONE', #9283, 1000.000000000000000 ) ;
#4592 = CARTESIAN_POINT ( 'NONE',  ( -10.25088531517539714, 30.80589556422609832, 83.57661607529820458 ) ) ;
#4593 = DIRECTION ( 'NONE',  ( 0.000000000000000000, 0.000000000000000000, -1.000000000000000000 ) ) ;
#4594 = ORIENTED_EDGE ( 'NONE', *, *, #4685, .T. ) ;
#4595 = CARTESIAN_POINT ( 'NONE',  ( 79.82136590429890077, 114.1051029460540605, 20.00000000000000000 ) ) ;
#4596 = EDGE_LOOP ( 'NONE', ( #2791, #7136, #2642, #9318 ) ) ;
#4597 = DIRECTION ( 'NONE',  ( 0.000000000000000000, 0.000000000000000000, 1.000000000000000000 ) ) ;
#4598 = DIRECTION ( 'NONE',  ( 0.000000000000000000, 0.000000000000000000, 1.000000000000000000 ) ) ;
#4599 = CARTESIAN_POINT ( 'NONE',  ( 111.0903281124166710, 100.8715034839261762, 20.00000000000000000 ) ) ;
#4600 = DIRECTION ( 'NONE',  ( 0.000000000000000000, 0.000000000000000000, 1.000000000000000000 ) ) ;
#4601 = MANIFOLD_SOLID_BREP ( 'NONE', #2135 ) ;
#4602 = CARTESIAN_POINT ( 'NONE',  ( -10.47404583389237942, 25.90703532196704728, 58.54999999999999716 ) ) ;
#4603 = DIRECTION ( 'NONE',  ( 0.000000000000000000, 0.000000000000000000, 1.000000000000000000 ) ) ;
#4604 = EDGE_CURVE ( 'NONE', #10154, #318, #10820, .T. ) ;
#4605 = CIRCLE ( 'NONE', #7695, 3.500000000000000888 ) ;
#4606 = CARTESIAN_POINT ( 'NONE',  ( 43.38563590245419732, 87.34974178189119698, 0.000000000000000000 ) ) ;
#4607 = CARTESIAN_POINT ( 'NONE',  ( -1.059188295049996231, -6.027090492554000534, 58.85000000000000142 ) ) ;
#4608 = EDGE_CURVE ( 'NONE', #859, #4292, #3186, .T. ) ;
#4609 = ADVANCED_FACE ( 'NONE', ( #5289, #8640 ), #2248, .T. ) ;
#4610 = ORIENTED_EDGE ( 'NONE', *, *, #11933, .T. ) ;
#4611 = CIRCLE ( 'NONE', #7046, 6.449999999999997513 ) ;
#4612 = VERTEX_POINT ( 'NONE', #3160 ) ;
#4613 = CARTESIAN_POINT ( 'NONE',  ( -24.37001676333060018, -4.028726038184999858, 62.14999999999999858 ) ) ;
#4614 = EDGE_LOOP ( 'NONE', ( #9688, #8963, #3032, #756 ) ) ;
#4615 = ORIENTED_EDGE ( 'NONE', *, *, #3726, .F. ) ;
#4616 = CARTESIAN_POINT ( 'NONE',  ( -16.64497473267689998, 26.91028695795525039, 56.84999999999999432 ) ) ;
#4617 = DIRECTION ( 'NONE',  ( 0.000000000000000000, 0.000000000000000000, -1.000000000000000000 ) ) ;
#4618 = DIRECTION ( 'NONE',  ( -0.000000000000000000, -0.000000000000000000, -1.000000000000000000 ) ) ;
#4619 = DIRECTION ( 'NONE',  ( 0.000000000000000000, 0.000000000000000000, 1.000000000000000000 ) ) ;
#4620 = CARTESIAN_POINT ( 'NONE',  ( -10.25088531517542023, -8.860076549334110041, 5.250000000000000000 ) ) ;
#4621 = AXIS2_PLACEMENT_3D ( 'NONE', #11803, #12914, #2262 ) ;
#4622 = CARTESIAN_POINT ( 'NONE',  ( 0.000000000000000000, 4.500000000000000000, 0.000000000000000000 ) ) ;
#4623 = ADVANCED_FACE ( 'NONE', ( #2044 ), #6485, .F. ) ;
#4624 = ORIENTED_EDGE ( 'NONE', *, *, #5706, .T. ) ;
#4625 = ORIENTED_EDGE ( 'NONE', *, *, #7940, .F. ) ;
#4626 = CARTESIAN_POINT ( 'NONE',  ( -17.49469255251400313, 30.35356550733773062, 61.66211139510344452 ) ) ;
#4627 = VERTEX_POINT ( 'NONE', #6284 ) ;
#4628 = EDGE_LOOP ( 'NONE', ( #1876, #3246 ) ) ;
#4629 = STYLED_ITEM ( 'NONE', ( #11094 ), #9410 ) ;
#4630 = ORIENTED_EDGE ( 'NONE', *, *, #5690, .T. ) ;
#4631 = CARTESIAN_POINT ( 'NONE',  ( 16.04064420431708982, 4.500000000000000000, 9.307586582922137808 ) ) ;
#4632 = DIRECTION ( 'NONE',  ( 0.000000000000000000, 0.000000000000000000, 1.000000000000000000 ) ) ;
#4633 = ORIENTED_EDGE ( 'NONE', *, *, #12966, .F. ) ;
#4634 = CARTESIAN_POINT ( 'NONE',  ( -18.45469220996244886, -1.832421873814834123, 0.000000000000000000 ) ) ;
#4635 = CARTESIAN_POINT ( 'NONE',  ( -27.15409092487699994, 0.3335619008453594714, 62.14999999999999858 ) ) ;
#4636 = PLANE ( 'NONE',  #5781 ) ;
#4637 = DIRECTION ( 'NONE',  ( 0.000000000000000000, 0.000000000000000000, 1.000000000000000000 ) ) ;
#4638 = VECTOR ( 'NONE', #11220, 1000.000000000000114 ) ;
#4639 = AXIS2_PLACEMENT_3D ( 'NONE', #173, #1220, #9689 ) ;
#4640 =( GEOMETRIC_REPRESENTATION_CONTEXT ( 3 ) GLOBAL_UNCERTAINTY_ASSIGNED_CONTEXT ( ( #6697 ) ) GLOBAL_UNIT_ASSIGNED_CONTEXT ( ( #9613, #13787, #4241 ) ) REPRESENTATION_CONTEXT ( 'NONE', 'WORKASPACE' ) );
#4641 = EDGE_LOOP ( 'NONE', ( #6738, #116, #2433, #741 ) ) ;
#4642 = ORIENTED_EDGE ( 'NONE', *, *, #4456, .F. ) ;
#4643 = EDGE_CURVE ( 'NONE', #4661, #7731, #4951, .T. ) ;
#4644 = ORIENTED_EDGE ( 'NONE', *, *, #4953, .F. ) ;
#4645 = EDGE_LOOP ( 'NONE', ( #6622, #5722, #8597, #1606 ) ) ;
#4646 = EDGE_CURVE ( 'NONE', #997, #11352, #7841, .T. ) ;
#4647 = ORIENTED_EDGE ( 'NONE', *, *, #3225, .T. ) ;
#4648 = DIRECTION ( 'NONE',  ( 0.000000000000000000, 0.000000000000000000, -1.000000000000000000 ) ) ;
#4649 = AXIS2_PLACEMENT_3D ( 'NONE', #1455, #1597, #10132 ) ;
#4650 = CIRCLE ( 'NONE', #7747, 16.72262947720610171 ) ;
#4651 = VERTEX_POINT ( 'NONE', #9495 ) ;
#4652 = CARTESIAN_POINT ( 'NONE',  ( -37.75918829505000218, 27.97290950744599769, 64.85000000000000853 ) ) ;
#4653 = AXIS2_PLACEMENT_3D ( 'NONE', #7760, #7681, #12175 ) ;
#4654 = CARTESIAN_POINT ( 'NONE',  ( -21.35558781198856337, 30.12521254561496775, 59.55915808916093113 ) ) ;
#4655 = DIRECTION ( 'NONE',  ( -0.6615960714621569316, 0.7498604124941125049, 0.000000000000000000 ) ) ;
#4656 = DIRECTION ( 'NONE',  ( 0.000000000000000000, 0.000000000000000000, -1.000000000000000000 ) ) ;
#4657 = DIRECTION ( 'NONE',  ( 0.000000000000000000, 0.000000000000000000, -1.000000000000000000 ) ) ;
#4658 = DIRECTION ( 'NONE',  ( 1.000000000000000000, 3.614007241618347908E-17, 0.000000000000000000 ) ) ;
#4659 = CARTESIAN_POINT ( 'NONE',  ( -18.05918829504999934, 10.97290950744599947, 64.85000000000000853 ) ) ;
#4660 =( LENGTH_UNIT ( ) NAMED_UNIT ( * ) SI_UNIT ( .MILLI., .METRE. ) );
#4661 = VERTEX_POINT ( 'NONE', #8511 ) ;
#4662 = ORIENTED_EDGE ( 'NONE', *, *, #9969, .F. ) ;
#4663 = AXIS2_PLACEMENT_3D ( 'NONE', #4298, #7459, #10784 ) ;
#4664 = CIRCLE ( 'NONE', #4440, 4.250000000000000000 ) ;
#4665 = AXIS2_PLACEMENT_3D ( 'NONE', #10191, #6893, #7936 ) ;
#4666 = ORIENTED_EDGE ( 'NONE', *, *, #12732, .F. ) ;
#4667 = EDGE_CURVE ( 'NONE', #4388, #10924, #6409, .T. ) ;
#4668 = LINE ( 'NONE', #13040, #1464 ) ;
#4669 = CARTESIAN_POINT ( 'NONE',  ( -18.05918829504999934, 10.97290950744599947, 63.64999999999999858 ) ) ;
#4670 = EDGE_CURVE ( 'NONE', #6829, #9069, #943, .T. ) ;
#4671 = DIRECTION ( 'NONE',  ( 0.000000000000000000, 0.000000000000000000, 1.000000000000000000 ) ) ;
#4672 = DIRECTION ( 'NONE',  ( -1.000000000000000000, -0.000000000000000000, -0.000000000000000000 ) ) ;
#4673 = PLANE ( 'NONE',  #5961 ) ;
#4674 = PLANE ( 'NONE',  #1577 ) ;
#4675 = CARTESIAN_POINT ( 'NONE',  ( 16.04064420431708982, 4.500000000000000000, 9.307586582922137808 ) ) ;
#4676 = ORIENTED_EDGE ( 'NONE', *, *, #1249, .T. ) ;
#4677 = CARTESIAN_POINT ( 'NONE',  ( -35.05918829505000645, 10.97290950744599947, 57.35000000000000142 ) ) ;
#4678 = CARTESIAN_POINT ( 'NONE',  ( -35.05918829505000645, -6.027090492554000534, 64.35000000000000853 ) ) ;
#4679 = CYLINDRICAL_SURFACE ( 'NONE', #1580, 1.999999999999986233 ) ;
#4680 = AXIS2_PLACEMENT_3D ( 'NONE', #6338, #11851, #259 ) ;
#4681 = PRODUCT_RELATED_PRODUCT_CATEGORY ( 'part', '', ( #5400 ) ) ;
#4682 = CARTESIAN_POINT ( 'NONE',  ( 134.6356359024541973, 89.90549801902423610, 23.00000000000000000 ) ) ;
#4683 = DIRECTION ( 'NONE',  ( -0.000000000000000000, 1.000000000000000000, -0.000000000000000000 ) ) ;
#4684 = ORIENTED_EDGE ( 'NONE', *, *, #10549, .T. ) ;
#4685 = EDGE_CURVE ( 'NONE', #10154, #5017, #1236, .T. ) ;
#4686 = ORIENTED_EDGE ( 'NONE', *, *, #3131, .F. ) ;
#4687 = AXIS2_PLACEMENT_3D ( 'NONE', #9527, #10719, #7411 ) ;
#4688 = EDGE_LOOP ( 'NONE', ( #12739, #7200, #3891, #1472 ) ) ;
#4689 = CARTESIAN_POINT ( 'NONE',  ( -18.05918829504999934, 10.97290950744599947, 62.14999999999999858 ) ) ;
#4690 = CIRCLE ( 'NONE', #5331, 34.69999999999999574 ) ;
#4691 = EDGE_LOOP ( 'NONE', ( #7048, #788, #13802, #13735, #10900 ) ) ;
#4692 = CARTESIAN_POINT ( 'NONE',  ( -18.05918829504999934, 10.97290950744599947, 64.85000000000000853 ) ) ;
#4693 = DIRECTION ( 'NONE',  ( 0.000000000000000000, 1.000000000000000000, 0.000000000000000000 ) ) ;
#4694 = FACE_OUTER_BOUND ( 'NONE', #3188, .T. ) ;
#4695 = PLANE ( 'NONE',  #8666 ) ;
#4696 = EDGE_CURVE ( 'NONE', #1212, #13218, #1833, .T. ) ;
#4697 = DIRECTION ( 'NONE',  ( 0.000000000000000000, 0.000000000000000000, 1.000000000000000000 ) ) ;
#4698 = CARTESIAN_POINT ( 'NONE',  ( 27.50000000000001066, 9.000000000000000000, 29.99999999999999645 ) ) ;
#4699 = VECTOR ( 'NONE', #6632, 1000.000000000000000 ) ;
#4700 = VECTOR ( 'NONE', #3671, 1000.000000000000000 ) ;
#4701 = ADVANCED_FACE ( 'NONE', ( #7935 ), #3692, .T. ) ;
#4702 = ORIENTED_EDGE ( 'NONE', *, *, #2361, .T. ) ;
#4703 = CARTESIAN_POINT ( 'NONE',  ( -18.05918829504999934, 10.97290950744599947, 27.30000000000000071 ) ) ;
#4704 = ORIENTED_EDGE ( 'NONE', *, *, #5555, .T. ) ;
#4705 = ORIENTED_EDGE ( 'NONE', *, *, #5867, .F. ) ;
#4706 = CONICAL_SURFACE ( 'NONE', #10723, 16.75000000000000355, 0.7853981633974461696 ) ;
#4707 = ORIENTED_EDGE ( 'NONE', *, *, #299, .F. ) ;
#4708 = VECTOR ( 'NONE', #5919, 1000.000000000000000 ) ;
#4709 = VECTOR ( 'NONE', #1405, 1000.000000000000000 ) ;
#4710 = AXIS2_PLACEMENT_3D ( 'NONE', #3430, #3105, #8858 ) ;
#4711 = CARTESIAN_POINT ( 'NONE',  ( -30.80918829504999934, -6.027090492554000534, 64.35000000000000853 ) ) ;
#4712 = LINE ( 'NONE', #1269, #7295 ) ;
#4713 = ADVANCED_FACE ( 'NONE', ( #11097 ), #9980, .F. ) ;
#4714 = DIRECTION ( 'NONE',  ( 0.000000000000000000, 0.000000000000000000, 1.000000000000000000 ) ) ;
#4715 = DIRECTION ( 'NONE',  ( 0.000000000000000000, 0.000000000000000000, -1.000000000000000000 ) ) ;
#4716 = LINE ( 'NONE', #12527, #13364 ) ;
#4717 = CARTESIAN_POINT ( 'NONE',  ( 1.640811704950000172, -6.027090492554000534, 64.85000000000000853 ) ) ;
#4718 = CIRCLE ( 'NONE', #9850, 16.66282263685194920 ) ;
#4719 = ORIENTED_EDGE ( 'NONE', *, *, #6603, .T. ) ;
#4720 = CIRCLE ( 'NONE', #11620, 18.00000000000000000 ) ;
#4721 = ORIENTED_EDGE ( 'NONE', *, *, #13638, .T. ) ;
#4722 = ORIENTED_EDGE ( 'NONE', *, *, #5194, .T. ) ;
#4723 = PLANE ( 'NONE',  #6385 ) ;
#4724 = VERTEX_POINT ( 'NONE', #5842 ) ;
#4725 = CARTESIAN_POINT ( 'NONE',  ( -21.63433128315409348, 30.08351321291810621, 58.90474581060517067 ) ) ;
#4726 = AXIS2_PLACEMENT_3D ( 'NONE', #991, #1251, #3441 ) ;
#4727 = AXIS2_PLACEMENT_3D ( 'NONE', #5125, #9399, #4991 ) ;
#4728 = PRESENTATION_STYLE_ASSIGNMENT (( #5621 ) ) ;
#4729 = PLANE ( 'NONE',  #7773 ) ;
#4730 = CIRCLE ( 'NONE', #931, 2.000000000000001776 ) ;
#4731 = CARTESIAN_POINT ( 'NONE',  ( -18.05918829358019906, 3.806800778008990083, 61.72253826514069885 ) ) ;
#4732 = CARTESIAN_POINT ( 'NONE',  ( -35.05918829505000645, 27.97290950744599769, 64.85000000000000853 ) ) ;
#4733 = DIRECTION ( 'NONE',  ( 0.000000000000000000, 0.000000000000000000, 1.000000000000000000 ) ) ;
#4734 = ADVANCED_FACE ( 'NONE', ( #2391 ), #11640, .T. ) ;
#4735 = AXIS2_PLACEMENT_3D ( 'NONE', #4539, #3427, #340 ) ;
#4736 = ORIENTED_EDGE ( 'NONE', *, *, #11455, .F. ) ;
#4737 = DIRECTION ( 'NONE',  ( -0.000000000000000000, -0.000000000000000000, 1.000000000000000000 ) ) ;
#4738 = FACE_BOUND ( 'NONE', #9437, .T. ) ;
#4739 = ORIENTED_EDGE ( 'NONE', *, *, #9499, .F. ) ;
#4740 = DIRECTION ( 'NONE',  ( -1.577021341797097560E-16, 1.000000000000000000, 0.000000000000000000 ) ) ;
#4741 = DIRECTION ( 'NONE',  ( 1.000000000000000000, 0.000000000000000000, 0.000000000000000000 ) ) ;
#4742 = DIRECTION ( 'NONE',  ( 0.000000000000000000, 0.000000000000000000, -1.000000000000000000 ) ) ;
#4743 = DIRECTION ( 'NONE',  ( 0.000000000000000000, 0.000000000000000000, -1.000000000000000000 ) ) ;
#4744 = DIRECTION ( 'NONE',  ( 0.000000000000000000, 0.000000000000000000, 1.000000000000000000 ) ) ;
#4745 = CARTESIAN_POINT ( 'NONE',  ( -12.87735031270726083, -6.265087914666309210, 62.14999999999999858 ) ) ;
#4746 = LINE ( 'NONE', #3568, #3539 ) ;
#4747 = CARTESIAN_POINT ( 'NONE',  ( -18.05918829504999934, 10.97290950744599947, 10.00000000000000000 ) ) ;
#4748 = AXIS2_PLACEMENT_3D ( 'NONE', #13589, #8295, #4043 ) ;
#4749 = CARTESIAN_POINT ( 'NONE',  ( 42.94629607423402007, 87.16776126655173584, 3.521624574640407997E-16 ) ) ;
#4750 = CARTESIAN_POINT ( 'NONE',  ( 44.63563590245423285, 113.0390816101113387, 0.3106601717798216367 ) ) ;
#4751 = ADVANCED_FACE ( 'NONE', ( #13112 ), #9000, .F. ) ;
#4752 = ORIENTED_EDGE ( 'NONE', *, *, #9264, .F. ) ;
#4753 = EDGE_LOOP ( 'NONE', ( #13039, #3467 ) ) ;
#4754 = CARTESIAN_POINT ( 'NONE',  ( -3.759188295049999518, 27.97290950744599769, 7.250000000000000000 ) ) ;
#4755 = VERTEX_POINT ( 'NONE', #8931 ) ;
#4756 = CARTESIAN_POINT ( 'NONE',  ( 1.940811704950003991, -6.027090492554000534, 0.000000000000000000 ) ) ;
#4757 = CARTESIAN_POINT ( 'NONE',  ( -5.309188295050000228, 27.97290950744599769, 64.35000000000000853 ) ) ;
#4758 = PRESENTATION_STYLE_ASSIGNMENT (( #556 ) ) ;
#4759 = CARTESIAN_POINT ( 'NONE',  ( -18.05918829504999934, 10.97290950744599947, 58.54999999999999716 ) ) ;
#4760 = CARTESIAN_POINT ( 'NONE',  ( -13.16523020061520022, -5.307421391215619622, 62.14999999999999858 ) ) ;
#4761 = APPLICATION_CONTEXT ( 'automotive_design' ) ;
#4762 = DIRECTION ( 'NONE',  ( 1.000000000000000000, 0.000000000000000000, -0.000000000000000000 ) ) ;
#4763 = EDGE_CURVE ( 'NONE', #8462, #2899, #2461, .T. ) ;
#4764 = DIRECTION ( 'NONE',  ( 0.000000000000000000, 0.000000000000000000, 1.000000000000000000 ) ) ;
#4765 = AXIS2_PLACEMENT_3D ( 'NONE', #3524, #8185, #12178 ) ;
#4766 = EDGE_CURVE ( 'NONE', #6439, #12616, #2297, .T. ) ;
#4767 = ORIENTED_EDGE ( 'NONE', *, *, #7843, .F. ) ;
#4768 = EDGE_CURVE ( 'NONE', #182, #2876, #6690, .T. ) ;
#4769 = CARTESIAN_POINT ( 'NONE',  ( -18.05918829504999934, 10.97290950744599947, 63.14999999999999858 ) ) ;
#4770 = ORIENTED_EDGE ( 'NONE', *, *, #4165, .T. ) ;
#4771 = ORIENTED_EDGE ( 'NONE', *, *, #9115, .F. ) ;
#4772 = ORIENTED_EDGE ( 'NONE', *, *, #6099, .T. ) ;
#4773 = CIRCLE ( 'NONE', #1645, 3.000000000000000000 ) ;
#4774 = ORIENTED_EDGE ( 'NONE', *, *, #10824, .F. ) ;
#4775 = FACE_OUTER_BOUND ( 'NONE', #13295, .T. ) ;
#4776 = CARTESIAN_POINT ( 'NONE',  ( -33.29928216905001648, 18.59295644444599915, 61.63595870799996845 ) ) ;
#4777 = DIRECTION ( 'NONE',  ( 1.000000000000000000, 0.000000000000000000, 0.000000000000000000 ) ) ;
#4778 = ORIENTED_EDGE ( 'NONE', *, *, #8616, .T. ) ;
#4779 = DIRECTION ( 'NONE',  ( -8.673617379884027583E-16, -1.000000000000000000, 0.000000000000000000 ) ) ;
#4780 = FACE_OUTER_BOUND ( 'NONE', #84, .T. ) ;
#4781 = CARTESIAN_POINT ( 'NONE',  ( -25.29804148384604900, -2.574630058508220021, 63.45000000000000284 ) ) ;
#4782 = EDGE_CURVE ( 'NONE', #10863, #7611, #10127, .T. ) ;
#4783 = DIRECTION ( 'NONE',  ( -1.000000000000000000, 0.000000000000000000, 0.000000000000000000 ) ) ;
#4784 = EDGE_CURVE ( 'NONE', #10025, #10920, #10307, .T. ) ;
#4785 = DIRECTION ( 'NONE',  ( -0.9496839325805417342, -0.3132098788326399541, 0.000000000000000000 ) ) ;
#4786 = ORIENTED_EDGE ( 'NONE', *, *, #5831, .T. ) ;
#4787 = DIRECTION ( 'NONE',  ( -0.6615960714621569316, 0.7498604124941123938, 0.000000000000000000 ) ) ;
#4788 = CARTESIAN_POINT ( 'NONE',  ( -21.27752276159345968, 30.13625835399255593, 54.99767865737477734 ) ) ;
#4789 = CARTESIAN_POINT ( 'NONE',  ( -35.05918829505000645, 27.97290950744599769, 58.85000000000000142 ) ) ;
#4790 = LINE ( 'NONE', #3680, #198 ) ;
#4791 = DIRECTION ( 'NONE',  ( 1.000000000000000000, 0.000000000000000000, 0.000000000000000000 ) ) ;
#4792 = DIRECTION ( 'NONE',  ( 0.000000000000000000, 0.000000000000000000, -1.000000000000000000 ) ) ;
#4793 = CARTESIAN_POINT ( 'NONE',  ( -34.05918829504999934, 10.97290950744599947, 56.84999999999999432 ) ) ;
#4794 = EDGE_CURVE ( 'NONE', #7262, #6072, #5637, .T. ) ;
#4795 = AXIS2_PLACEMENT_3D ( 'NONE', #12375, #564, #10281 ) ;
#4796 = CARTESIAN_POINT ( 'NONE',  ( -4.599650328638321461, 8.500000000000001776, -5.878124499050803919 ) ) ;
#4797 = CARTESIAN_POINT ( 'NONE',  ( -10.82033510625394079, -2.574630058508199593, 63.45000000000000284 ) ) ;
#4798 = ORIENTED_EDGE ( 'NONE', *, *, #8003, .F. ) ;
#4799 = DIRECTION ( 'NONE',  ( -0.4528443260392611136, -0.8915896008669277339, 0.000000000000000000 ) ) ;
#4800 =( NAMED_UNIT ( * ) PLANE_ANGLE_UNIT ( ) SI_UNIT ( $, .RADIAN. ) );
#4801 = CARTESIAN_POINT ( 'NONE',  ( -3.999999999999997335, 2.000000000000000000, -65.00000000000000000 ) ) ;
#4802 = CARTESIAN_POINT ( 'NONE',  ( 1.940811704950001770, 10.97290950744599947, 11.50000000000000000 ) ) ;
#4803 = DIRECTION ( 'NONE',  ( 0.000000000000000000, 0.000000000000000000, -1.000000000000000000 ) ) ;
#4804 = LINE ( 'NONE', #1726, #9566 ) ;
#4805 = CARTESIAN_POINT ( 'NONE',  ( 0.000000000000000000, 0.000000000000000000, 23.00000000000000000 ) ) ;
#4806 = FACE_OUTER_BOUND ( 'NONE', #4019, .T. ) ;
#4807 = DIRECTION ( 'NONE',  ( 1.000000000000000000, 0.000000000000000000, 0.000000000000000000 ) ) ;
#4808 = CIRCLE ( 'NONE', #10612, 1.999999999999986233 ) ;
#4809 = ADVANCED_FACE ( 'NONE', ( #3635 ), #9919, .T. ) ;
#4810 = ORIENTED_EDGE ( 'NONE', *, *, #6387, .T. ) ;
#4811 = ORIENTED_EDGE ( 'NONE', *, *, #3969, .F. ) ;
#4812 = CARTESIAN_POINT ( 'NONE',  ( 42.94629607423402007, 110.9104019536709842, 4.059660689008197386E-16 ) ) ;
#4813 = EDGE_CURVE ( 'NONE', #322, #10451, #2754, .T. ) ;
#4814 = EDGE_CURVE ( 'NONE', #1230, #3770, #13047, .T. ) ;
#4815 = ORIENTED_EDGE ( 'NONE', *, *, #1738, .T. ) ;
#4816 = ORIENTED_EDGE ( 'NONE', *, *, #3841, .T. ) ;
#4817 = CARTESIAN_POINT ( 'NONE',  ( -18.05918829504999934, 10.97290950744599947, 62.85000000000000142 ) ) ;
#4818 = CARTESIAN_POINT ( 'NONE',  ( 0.000000000000000000, 8.500000000000000000, 0.000000000000000000 ) ) ;
#4819 = FILL_AREA_STYLE ('',( #499 ) ) ;
#4820 = CARTESIAN_POINT ( 'NONE',  ( 140.3856359024541973, 94.65549801902425031, 23.00000000000000000 ) ) ;
#4821 = CARTESIAN_POINT ( 'NONE',  ( -18.05918829504999934, 10.97290950744599947, 27.09999999999999787 ) ) ;
#4822 = DIRECTION ( 'NONE',  ( 1.000000000000000000, 0.000000000000000000, 0.000000000000000000 ) ) ;
#4823 = CARTESIAN_POINT ( 'NONE',  ( -1.059188295049996231, -6.027090492554000534, 58.85000000000000142 ) ) ;
#4824 = CIRCLE ( 'NONE', #2846, 16.66282263685194920 ) ;
#4825 = VERTEX_POINT ( 'NONE', #2594 ) ;
#4826 = ORIENTED_EDGE ( 'NONE', *, *, #1528, .T. ) ;
#4827 = DIRECTION ( 'NONE',  ( 0.000000000000000000, 1.000000000000000000, 0.000000000000000000 ) ) ;
#4828 = VECTOR ( 'NONE', #7965, 1000.000000000000000 ) ;
#4829 = EDGE_CURVE ( 'NONE', #4386, #6747, #3490, .T. ) ;
#4830 = EDGE_LOOP ( 'NONE', ( #11463, #11345 ) ) ;
#4831 = DIRECTION ( 'NONE',  ( 0.000000000000000000, 0.000000000000000000, 1.000000000000000000 ) ) ;
#4832 = ORIENTED_EDGE ( 'NONE', *, *, #4222, .F. ) ;
#4833 = CARTESIAN_POINT ( 'NONE',  ( 50.63563590245420443, 89.90549801902423610, 20.00000000000000000 ) ) ;
#4834 = ADVANCED_FACE ( 'NONE', ( #7655, #481, #1309, #5567, #2662, #9857, #8856, #276, #12003, #3566 ), #12558, .F. ) ;
#4835 = PLANE ( 'NONE',  #630 ) ;
#4836 = DIRECTION ( 'NONE',  ( 0.000000000000000000, 0.000000000000000000, 1.000000000000000000 ) ) ;
#4837 = ORIENTED_EDGE ( 'NONE', *, *, #7216, .T. ) ;
#4838 = AXIS2_PLACEMENT_3D ( 'NONE', #7237, #1960, #6194 ) ;
#4839 = ADVANCED_FACE ( 'NONE', ( #10324 ), #49, .F. ) ;
#4840 = DIRECTION ( 'NONE',  ( -0.7071067811865524577, -0.7071067811865425767, 0.000000000000000000 ) ) ;
#4841 = DIRECTION ( 'NONE',  ( 1.000000000000000000, 0.000000000000000000, 0.000000000000000000 ) ) ;
#4842 = LINE ( 'NONE', #12329, #13152 ) ;
#4843 = DIRECTION ( 'NONE',  ( 0.000000000000000000, 0.000000000000000000, 1.000000000000000000 ) ) ;
#4844 = EDGE_LOOP ( 'NONE', ( #8143, #7144, #8830, #11108, #12047 ) ) ;
#4845 = AXIS2_PLACEMENT_3D ( 'NONE', #13455, #3899, #12410 ) ;
#4846 = ORIENTED_EDGE ( 'NONE', *, *, #2948, .T. ) ;
#4847 = ORIENTED_EDGE ( 'NONE', *, *, #10569, .T. ) ;
#4848 = EDGE_CURVE ( 'NONE', #7299, #12691, #4506, .T. ) ;
#4849 = EDGE_LOOP ( 'NONE', ( #9696, #82, #5965, #9368 ) ) ;
#4850 = CARTESIAN_POINT ( 'NONE',  ( 8.157609394192110841, 24.73469418910620021, 5.250000000000000000 ) ) ;
#4851 = ORIENTED_EDGE ( 'NONE', *, *, #1899, .T. ) ;
#4852 = DIRECTION ( 'NONE',  ( 0.000000000000000000, 1.672022627447524993E-15, 1.000000000000000000 ) ) ;
#4853 = EDGE_CURVE ( 'NONE', #11902, #4325, #8979, .T. ) ;
#4854 = CARTESIAN_POINT ( 'NONE',  ( -21.42523896548032880, 30.11514052156897847, 59.42030264396898787 ) ) ;
#4855 = AXIS2_PLACEMENT_3D ( 'NONE', #4303, #3057, #9674 ) ;
#4856 = DIRECTION ( 'NONE',  ( 1.000000000000000000, 0.000000000000000000, 0.000000000000000000 ) ) ;
#4857 = CARTESIAN_POINT ( 'NONE',  ( -39.30918829504999934, -6.027090492554000534, 64.35000000000000853 ) ) ;
#4858 = PLANE ( 'NONE',  #11636 ) ;
#4859 = CIRCLE ( 'NONE', #7076, 1.725000000000000755 ) ;
#4860 = EDGE_CURVE ( 'NONE', #159, #3998, #1940, .T. ) ;
#4861 = FACE_OUTER_BOUND ( 'NONE', #10850, .T. ) ;
#4862 = APPLICATION_PROTOCOL_DEFINITION ( 'draft international standard', 'automotive_design', 1998, #13135 ) ;
#4863 = ORIENTED_EDGE ( 'NONE', *, *, #12315, .T. ) ;
#4864 = AXIS2_PLACEMENT_3D ( 'NONE', #13681, #8169, #2888 ) ;
#4865 = EDGE_CURVE ( 'NONE', #11975, #8119, #13211, .T. ) ;
#4866 = ORIENTED_EDGE ( 'NONE', *, *, #9195, .T. ) ;
#4867 = AXIS2_PLACEMENT_3D ( 'NONE', #2422, #9809, #4632 ) ;
#4868 = CARTESIAN_POINT ( 'NONE',  ( 92.63563590245421153, 99.03908161011133870, 0.000000000000000000 ) ) ;
#4869 = FACE_OUTER_BOUND ( 'NONE', #11493, .T. ) ;
#4870 = ORIENTED_EDGE ( 'NONE', *, *, #9029, .F. ) ;
#4871 = DIRECTION ( 'NONE',  ( 1.000000000000000000, 0.000000000000000000, 0.000000000000000000 ) ) ;
#4872 = DIRECTION ( 'NONE',  ( 0.000000000000000000, 0.000000000000000000, -1.000000000000000000 ) ) ;
#4873 = DIRECTION ( 'NONE',  ( 0.000000000000000000, 0.000000000000000000, 1.000000000000000000 ) ) ;
#4874 = DIRECTION ( 'NONE',  ( -0.000000000000000000, -0.000000000000000000, -1.000000000000000000 ) ) ;
#4875 = CARTESIAN_POINT ( 'NONE',  ( -34.78181777225609750, 10.00028003023991907, 62.14999999999999858 ) ) ;
#4876 = CARTESIAN_POINT ( 'NONE',  ( 92.63563590245421153, 85.78908161011133870, 0.000000000000000000 ) ) ;
#4877 = LINE ( 'NONE', #10456, #7314 ) ;
#4878 = CARTESIAN_POINT ( 'NONE',  ( -18.05918829504999934, 10.97290950744599947, 7.250000000000000000 ) ) ;
#4879 = EDGE_CURVE ( 'NONE', #2779, #3533, #960, .T. ) ;
#4880 = FACE_OUTER_BOUND ( 'NONE', #3039, .T. ) ;
#4881 = DIRECTION ( 'NONE',  ( 0.000000000000000000, 0.000000000000000000, -1.000000000000000000 ) ) ;
#4882 = AXIS2_PLACEMENT_3D ( 'NONE', #2467, #1391, #2667 ) ;
#4883 = CIRCLE ( 'NONE', #1523, 3.450000000000001510 ) ;
#4884 = VECTOR ( 'NONE', #1237, 1000.000000000000000 ) ;
#4885 = VECTOR ( 'NONE', #2061, 1000.000000000000000 ) ;
#4886 = ORIENTED_EDGE ( 'NONE', *, *, #12780, .F. ) ;
#4887 = ORIENTED_EDGE ( 'NONE', *, *, #2326, .T. ) ;
#4888 = CARTESIAN_POINT ( 'NONE',  ( 44.88563590245420443, 90.15549801902423610, 23.00000000000000000 ) ) ;
#4889 = ORIENTED_EDGE ( 'NONE', *, *, #381, .F. ) ;
#4890 = AXIS2_PLACEMENT_3D ( 'NONE', #7519, #6430, #10910 ) ;
#4891 = AXIS2_PLACEMENT_3D ( 'NONE', #1157, #1021, #6469 ) ;
#4892 = ORIENTED_EDGE ( 'NONE', *, *, #2948, .F. ) ;
#4893 = CARTESIAN_POINT ( 'NONE',  ( 1.640811704950000172, 27.97290950744599769, 58.85000000000000142 ) ) ;
#4894 = AXIS2_PLACEMENT_3D ( 'NONE', #6181, #6053, #747 ) ;
#4895 = DIRECTION ( 'NONE',  ( -0.000000000000000000, -0.000000000000000000, 1.000000000000000000 ) ) ;
#4896 = DIRECTION ( 'NONE',  ( 0.000000000000000000, 0.000000000000000000, 1.000000000000000000 ) ) ;
#4897 = DIRECTION ( 'NONE',  ( -1.000000000000000000, 0.000000000000000000, 0.000000000000000000 ) ) ;
#4898 = DIRECTION ( 'NONE',  ( -1.000000000000000000, 0.000000000000000000, 0.000000000000000000 ) ) ;
#4899 = CARTESIAN_POINT ( 'NONE',  ( -17.23821357112329977, 5.029341513162310484, 67.84999999999999432 ) ) ;
#4900 = CARTESIAN_POINT ( 'NONE',  ( -1.396365658198039927, 10.97290950744599947, 17.25000000000000000 ) ) ;
#4901 = EDGE_CURVE ( 'NONE', #7761, #1281, #12933, .T. ) ;
#4902 = AXIS2_PLACEMENT_3D ( 'NONE', #1631, #9947, #12043 ) ;
#4903 = AXIS2_PLACEMENT_3D ( 'NONE', #5551, #532, #12195 ) ;
#4904 = VERTEX_POINT ( 'NONE', #13520 ) ;
#4905 = FACE_OUTER_BOUND ( 'NONE', #13073, .T. ) ;
#4906 = ORIENTED_EDGE ( 'NONE', *, *, #4090, .T. ) ;
#4907 = ORIENTED_EDGE ( 'NONE', *, *, #3469, .F. ) ;
#4908 = CARTESIAN_POINT ( 'NONE',  ( -12.81426999815532497, 15.06602133594271820, 0.000000000000000000 ) ) ;
#4909 = FACE_OUTER_BOUND ( 'NONE', #10314, .T. ) ;
#4910 = FACE_OUTER_BOUND ( 'NONE', #11526, .T. ) ;
#4911 = FACE_OUTER_BOUND ( 'NONE', #9203, .T. ) ;
#4912 = CARTESIAN_POINT ( 'NONE',  ( 44.88563590245420443, 108.9054980190242503, 22.75000000000000000 ) ) ;
#4913 = AXIS2_PLACEMENT_3D ( 'NONE', #4669, #601, #7862 ) ;
#4914 = DIRECTION ( 'NONE',  ( 1.000000000000000000, 0.000000000000000000, 0.000000000000000000 ) ) ;
#4915 = AXIS2_PLACEMENT_3D ( 'NONE', #10791, #1206, #5460 ) ;
#4916 = DIRECTION ( 'NONE',  ( -1.000000000000000000, 0.000000000000000000, 0.000000000000000000 ) ) ;
#4917 = FACE_OUTER_BOUND ( 'NONE', #13215, .T. ) ;
#4918 = EDGE_CURVE ( 'NONE', #1530, #6060, #7177, .T. ) ;
#4919 = AXIS2_PLACEMENT_3D ( 'NONE', #11709, #9684, #9611 ) ;
#4920 = AXIS2_PLACEMENT_3D ( 'NONE', #12641, #5162, #11666 ) ;
#4921 = AXIS2_PLACEMENT_3D ( 'NONE', #9456, #13, #3185 ) ;
#4922 = DIRECTION ( 'NONE',  ( -0.4528443260392609471, -0.8915896008669278450, 0.000000000000000000 ) ) ;
#4923 = CARTESIAN_POINT ( 'NONE',  ( -43.05918829505002066, 32.97290950744599769, 0.000000000000000000 ) ) ;
#4924 = FACE_OUTER_BOUND ( 'NONE', #9763, .T. ) ;
#4925 = DIRECTION ( 'NONE',  ( -1.000000000000000000, -2.529805069132845816E-16, -0.000000000000000000 ) ) ;
#4926 = DIRECTION ( 'NONE',  ( -1.000000000000000000, 0.000000000000000000, 0.000000000000000000 ) ) ;
#4927 = DIRECTION ( 'NONE',  ( -0.7050191076322684935, 0.7091883091770476710, 0.000000000000000000 ) ) ;
#4928 = VECTOR ( 'NONE', #3204, 1000.000000000000227 ) ;
#4929 = CIRCLE ( 'NONE', #12736, 0.5000000000000004441 ) ;
#4930 = PRODUCT_CONTEXT ( 'NONE', #13135, 'mechanical' ) ;
#4931 = VECTOR ( 'NONE', #9276, 1000.000000000000000 ) ;
#4932 = EDGE_LOOP ( 'NONE', ( #142, #6301, #12927, #2197 ) ) ;
#4933 = EDGE_CURVE ( 'NONE', #1569, #7689, #10316, .T. ) ;
#4934 = EDGE_CURVE ( 'NONE', #5535, #1130, #1657, .T. ) ;
#4935 = CARTESIAN_POINT ( 'NONE',  ( -19.47340185742309870, 26.91028695795525039, 56.84999999999999432 ) ) ;
#4936 = AXIS2_PLACEMENT_3D ( 'NONE', #10531, #11574, #671 ) ;
#4937 = ORIENTED_EDGE ( 'NONE', *, *, #2064, .T. ) ;
#4938 = VECTOR ( 'NONE', #3393, 1000.000000000000000 ) ;
#4939 = VERTEX_POINT ( 'NONE', #5905 ) ;
#4940 = DIRECTION ( 'NONE',  ( -0.7071067811865474617, 8.659560562354903276E-17, 0.7071067811865474617 ) ) ;
#4941 = CARTESIAN_POINT ( 'NONE',  ( 50.63563590245420443, 94.90549801902425031, 23.00000000000000000 ) ) ;
#4942 = DIRECTION ( 'NONE',  ( 1.000000000000000000, -1.679942734630170865E-14, 0.000000000000000000 ) ) ;
#4943 = DIRECTION ( 'NONE',  ( -0.000000000000000000, -0.000000000000000000, 1.000000000000000000 ) ) ;
#4944 = CARTESIAN_POINT ( 'NONE',  ( 8.000000000000001776, 2.000000000000000000, 0.000000000000000000 ) ) ;
#4945 = CARTESIAN_POINT ( 'NONE',  ( -1.336558817843898073, 10.00028003023991907, 62.14999999999999858 ) ) ;
#4946 = LINE ( 'NONE', #13462, #9798 ) ;
#4947 = CARTESIAN_POINT ( 'NONE',  ( -18.88016301897669891, 16.91647750172969822, 67.84999999999999432 ) ) ;
#4948 = CARTESIAN_POINT ( 'NONE',  ( -18.05918829504999934, 10.00028003023991907, 63.45000000000000284 ) ) ;
#4949 =( LENGTH_UNIT ( ) NAMED_UNIT ( * ) SI_UNIT ( .MILLI., .METRE. ) );
#4950 = EDGE_CURVE ( 'NONE', #2935, #7296, #2941, .T. ) ;
#4951 = CIRCLE ( 'NONE', #9191, 6.000000000000000888 ) ;
#4952 = VERTEX_POINT ( 'NONE', #9135 ) ;
#4953 = EDGE_CURVE ( 'NONE', #7844, #5689, #5071, .T. ) ;
#4954 = ORIENTED_EDGE ( 'NONE', *, *, #11649, .T. ) ;
#4955 = ORIENTED_EDGE ( 'NONE', *, *, #11492, .T. ) ;
#4956 = PLANE ( 'NONE',  #8585 ) ;
#4957 = ORIENTED_EDGE ( 'NONE', *, *, #10912, .F. ) ;
#4958 = ORIENTED_EDGE ( 'NONE', *, *, #7488, .F. ) ;
#4959 = DIRECTION ( 'NONE',  ( 1.000000000000000000, 0.000000000000000000, 0.000000000000000000 ) ) ;
#4960 = AXIS2_PLACEMENT_3D ( 'NONE', #2372, #8774, #4655 ) ;
#4961 = DIRECTION ( 'NONE',  ( 0.9496839325805427334, 0.3132098788326367345, 0.000000000000000000 ) ) ;
#4962 = CARTESIAN_POINT ( 'NONE',  ( 3.940811704950010430, -11.02709049255400053, 10.00000000000000000 ) ) ;
#4963 = LINE ( 'NONE', #4195, #10896 ) ;
#4964 = LINE ( 'NONE', #10280, #5795 ) ;
#4965 = CYLINDRICAL_SURFACE ( 'NONE', #8141, 9.999999999999994671 ) ;
#4966 = VECTOR ( 'NONE', #4568, 1000.000000000000000 ) ;
#4967 = ORIENTED_EDGE ( 'NONE', *, *, #12273, .T. ) ;
#4968 = EDGE_CURVE ( 'NONE', #4364, #4458, #13388, .T. ) ;
#4969 = ORIENTED_EDGE ( 'NONE', *, *, #986, .T. ) ;
#4970 = CARTESIAN_POINT ( 'NONE',  ( -15.30684414934278337, 30.19664696495205902, 60.37107827764424428 ) ) ;
#4971 = ORIENTED_EDGE ( 'NONE', *, *, #3572, .F. ) ;
#4972 = DIRECTION ( 'NONE',  ( 0.000000000000000000, 0.000000000000000000, -1.000000000000000000 ) ) ;
#4973 = ORIENTED_EDGE ( 'NONE', *, *, #13674, .F. ) ;
#4974 = DIRECTION ( 'NONE',  ( -0.7050191076322684935, 0.7091883091770476710, 0.000000000000000000 ) ) ;
#4975 = CARTESIAN_POINT ( 'NONE',  ( -18.05918829504999934, 10.97290950744599947, 61.72253826518770836 ) ) ;
#4976 = ORIENTED_EDGE ( 'NONE', *, *, #3526, .F. ) ;
#4977 = DIRECTION ( 'NONE',  ( 0.4528443260392608916, 0.8915896008669277339, 0.000000000000000000 ) ) ;
#4978 = AXIS2_PLACEMENT_3D ( 'NONE', #13354, #12328, #2775 ) ;
#4979 = DIRECTION ( 'NONE',  ( -1.000000000000000000, 0.000000000000000000, 0.000000000000000000 ) ) ;
#4980 = CARTESIAN_POINT ( 'NONE',  ( -24.37001676333060018, -4.028726038184999858, 63.45000000000000284 ) ) ;
#4981 = CARTESIAN_POINT ( 'NONE',  ( 101.4499059006094512, 83.97306027416853169, 20.00000000000000000 ) ) ;
#4982 = VERTEX_POINT ( 'NONE', #7090 ) ;
#4983 = AXIS2_PLACEMENT_3D ( 'NONE', #10267, #9343, #1662 ) ;
#4984 = ORIENTED_EDGE ( 'NONE', *, *, #11704, .F. ) ;
#4985 = VERTEX_POINT ( 'NONE', #4944 ) ;
#4986 = VERTEX_POINT ( 'NONE', #9209 ) ;
#4987 = EDGE_CURVE ( 'NONE', #87, #6052, #13459, .T. ) ;
#4988 = ORIENTED_EDGE ( 'NONE', *, *, #5382, .T. ) ;
#4989 = EDGE_CURVE ( 'NONE', #12460, #4495, #3072, .T. ) ;
#4990 = DIRECTION ( 'NONE',  ( -1.000000000000000000, 0.000000000000000000, 0.000000000000000000 ) ) ;
#4991 = DIRECTION ( 'NONE',  ( 0.000000000000000000, 1.000000000000000000, 2.202823461557851130E-15 ) ) ;
#4992 = CARTESIAN_POINT ( 'NONE',  ( -18.05918829504999934, 10.97290950744599947, 60.65000000000000568 ) ) ;
#4993 = DIRECTION ( 'NONE',  ( 1.000000000000000000, 0.000000000000000000, 0.000000000000000000 ) ) ;
#4994 = DIRECTION ( 'NONE',  ( 1.000000000000000000, 0.000000000000000000, 0.000000000000000000 ) ) ;
#4995 = CYLINDRICAL_SURFACE ( 'NONE', #3786, 1.999999999999991340 ) ;
#4996 =( LENGTH_UNIT ( ) NAMED_UNIT ( * ) SI_UNIT ( .MILLI., .METRE. ) );
#4997 = VERTEX_POINT ( 'NONE', #10532 ) ;
#4998 = ORIENTED_EDGE ( 'NONE', *, *, #10096, .T. ) ;
#4999 = DIRECTION ( 'NONE',  ( -0.000000000000000000, -0.000000000000000000, 1.000000000000000000 ) ) ;
#5000 = VERTEX_POINT ( 'NONE', #7480 ) ;
#5001 = FACE_OUTER_BOUND ( 'NONE', #11172, .T. ) ;
#5002 = EDGE_CURVE ( 'NONE', #12622, #3976, #9201, .T. ) ;
#5003 = CARTESIAN_POINT ( 'NONE',  ( -24.20502162805000168, 10.97290950744599947, 61.10999999999999943 ) ) ;
#5004 = PLANE ( 'NONE',  #4281 ) ;
#5005 = ORIENTED_EDGE ( 'NONE', *, *, #10479, .F. ) ;
#5006 = DIRECTION ( 'NONE',  ( 0.000000000000000000, 0.000000000000000000, -1.000000000000000000 ) ) ;
#5007 = CARTESIAN_POINT ( 'NONE',  ( -18.05918829504999934, 10.97290950744599947, 60.04999999999999716 ) ) ;
#5008 = DIRECTION ( 'NONE',  ( 1.000000000000000000, 0.000000000000000000, 0.000000000000000000 ) ) ;
#5009 = LINE ( 'NONE', #5074, #4931 ) ;
#5010 = CARTESIAN_POINT ( 'NONE',  ( 44.63563590245422574, 113.0390816101113387, 0.7500000000000006661 ) ) ;
#5011 = EDGE_CURVE ( 'NONE', #2929, #3628, #4527, .T. ) ;
#5012 = PRODUCT_DEFINITION_CONTEXT ( 'detailed design', #4761, 'design' ) ;
#5013 = AXIS2_PLACEMENT_3D ( 'NONE', #8534, #1195, #2348 ) ;
#5014 =( REPRESENTATION_RELATIONSHIP ('NONE','NONE', #11848, #5502 ) REPRESENTATION_RELATIONSHIP_WITH_TRANSFORMATION ( #9603 )SHAPE_REPRESENTATION_RELATIONSHIP( ) );
#5015 = ORIENTED_EDGE ( 'NONE', *, *, #6711, .T. ) ;
#5016 = ORIENTED_EDGE ( 'NONE', *, *, #332, .T. ) ;
#5018 = ADVANCED_FACE ( 'NONE', ( #11575 ), #12621, .F. ) ;
#5017 = VERTEX_POINT ( 'NONE', #4174 ) ;
#5019 = FACE_OUTER_BOUND ( 'NONE', #1711, .T. ) ;
#5020 = CARTESIAN_POINT ( 'NONE',  ( -0.3963656581980404825, 10.97290950744599947, 7.250000000000000000 ) ) ;
#5021 = DIRECTION ( 'NONE',  ( 0.000000000000000000, 0.000000000000000000, -1.000000000000000000 ) ) ;
#5022 = CIRCLE ( 'NONE', #13717, 1.999999999999993117 ) ;
#5023 = PLANE ( 'NONE',  #8650 ) ;
#5024 = DIRECTION ( 'NONE',  ( 1.000000000000000000, 0.000000000000000000, 0.000000000000000000 ) ) ;
#5025 = EDGE_CURVE ( 'NONE', #11045, #4627, #2302, .T. ) ;
#5026 = VECTOR ( 'NONE', #13624, 1000.000000000000000 ) ;
#5027 = EDGE_LOOP ( 'NONE', ( #1358, #6130, #5340, #12715 ) ) ;
#5028 = CIRCLE ( 'NONE', #9723, 2.800000000000000266 ) ;
#5029 = ORIENTED_EDGE ( 'NONE', *, *, #9844, .T. ) ;
#5030 = CARTESIAN_POINT ( 'NONE',  ( -14.93961223533927729, 30.15001770392374070, 54.82814931419168403 ) ) ;
#5031 = ORIENTED_EDGE ( 'NONE', *, *, #9459, .F. ) ;
#5032 = CARTESIAN_POINT ( 'NONE',  ( 140.3856359024541973, 90.15549801902423610, 23.00000000000000000 ) ) ;
#5033 = DIRECTION ( 'NONE',  ( 0.000000000000000000, 0.000000000000000000, -1.000000000000000000 ) ) ;
#5034 = EDGE_LOOP ( 'NONE', ( #9608, #5463, #1029, #1123 ) ) ;
#5035 = CARTESIAN_POINT ( 'NONE',  ( -41.50918829505000218, 27.97290950744599769, 5.250000000000000000 ) ) ;
#5036 = PLANE ( 'NONE',  #3996 ) ;
#5037 = DIRECTION ( 'NONE',  ( 0.9496839325805410681, 0.3132098788326420080, 0.000000000000000000 ) ) ;
#5038 = DIRECTION ( 'NONE',  ( -1.000000000000000000, 0.000000000000000000, 0.000000000000000000 ) ) ;
#5039 = CARTESIAN_POINT ( 'NONE',  ( -5.309188295050000228, -6.027090492554000534, 58.85000000000000142 ) ) ;
#5040 = AXIS2_PLACEMENT_3D ( 'NONE', #12683, #7474, #9474 ) ;
#5041 = EDGE_CURVE ( 'NONE', #13769, #9617, #10103, .T. ) ;
#5042 = CARTESIAN_POINT ( 'NONE',  ( -40.05918829505000645, 32.97290950744599769, 0.000000000000000000 ) ) ;
#5043 = ORIENTED_EDGE ( 'NONE', *, *, #7984, .T. ) ;
#5044 = ORIENTED_EDGE ( 'NONE', *, *, #2342, .T. ) ;
#5045 = ORIENTED_EDGE ( 'NONE', *, *, #5268, .T. ) ;
#5046 = AXIS2_PLACEMENT_3D ( 'NONE', #8307, #7106, #9224 ) ;
#5047 = ORIENTED_EDGE ( 'NONE', *, *, #6310, .F. ) ;
#5048 = ORIENTED_EDGE ( 'NONE', *, *, #1465, .T. ) ;
#5049 = EDGE_LOOP ( 'NONE', ( #1304, #3911, #5591, #1634 ) ) ;
#5050 = DIRECTION ( 'NONE',  ( 1.000000000000000000, 0.000000000000000000, -0.000000000000000000 ) ) ;
#5051 = CARTESIAN_POINT ( 'NONE',  ( -19.35259110363697488, 30.32455137612451068, 61.45271661549876541 ) ) ;
#5052 = DIRECTION ( 'NONE',  ( 0.000000000000000000, 0.000000000000000000, 1.000000000000000000 ) ) ;
#5053 = DIRECTION ( 'NONE',  ( -0.000000000000000000, -0.000000000000000000, -1.000000000000000000 ) ) ;
#5054 = CARTESIAN_POINT ( 'NONE',  ( -18.05918829504999934, 10.97290950744599947, 62.14999999999999858 ) ) ;
#5055 = DIRECTION ( 'NONE',  ( -0.7091883091770476710, -0.7050191076322684935, 0.000000000000000000 ) ) ;
#5056 =( NAMED_UNIT ( * ) SI_UNIT ( $, .STERADIAN. ) SOLID_ANGLE_UNIT ( ) );
#5057 = ORIENTED_EDGE ( 'NONE', *, *, #3739, .F. ) ;
#5058 = VERTEX_POINT ( 'NONE', #103 ) ;
#5059 = VECTOR ( 'NONE', #4872, 1000.000000000000000 ) ;
#5060 = ADVANCED_FACE ( 'NONE', ( #9480 ), #6740, .F. ) ;
#5061 = EDGE_CURVE ( 'NONE', #3451, #665, #5846, .T. ) ;
#5062 = SHAPE_REPRESENTATION ( 'Adapter Flange Plate', ( #6434 ), #4214 ) ;
#5063 = CARTESIAN_POINT ( 'NONE',  ( -10.25088531517539892, 30.80589556422609832, 17.25000000000000000 ) ) ;
#5064 = ORIENTED_EDGE ( 'NONE', *, *, #5921, .T. ) ;
#5065 = CLOSED_SHELL ( 'NONE', ( #139, #1106, #8862, #11505, #13732, #4287, #13440, #2673, #6378, #4489, #6270, #2742, #7506, #5401, #10149, #13359, #9282, #6736, #10796, #7694, #6156, #1923, #12386, #11917, #10833, #6836, #7818, #7661, #12926, #7671, #2847, #3416, #2650, #1013, #3354, #4245, #6456, #5779, #521, #7582, #5577, #2094, #13208, #13464, #11511, #9551, #6968, #10720, #8743, #2129, #2794, #1739, #632, #7127, #7063, #12830, #5426, #7896, #1426, #13032, #2055, #7670, #5741, #4540, #12546, #3486, #10423, #4839, #3081, #7801, #5184, #3414, #4809, #9003, #9293, #6691, #7135, #7044, #7065, #7755, #8724, #8781, #3587, #1665, #7762, #1543, #4623, #1761, #5494, #3162, #2217, #3116, #9350, #13291, #13683, #7784, #3305, #1936, #7887 ) ) ;
#5066 = ORIENTED_EDGE ( 'NONE', *, *, #2914, .F. ) ;
#5067 = CARTESIAN_POINT ( 'NONE',  ( -11.91335496205000055, 10.97290950744599947, 61.10999999999999943 ) ) ;
#5068 = LINE ( 'NONE', #4941, #9076 ) ;
#5069 = AXIS2_PLACEMENT_3D ( 'NONE', #10973, #6819, #10052 ) ;
#5070 = CARTESIAN_POINT ( 'NONE',  ( -24.40502162805000097, 10.97290950744599947, 60.40999999999999659 ) ) ;
#5071 = LINE ( 'NONE', #10190, #8076 ) ;
#5072 = DIRECTION ( 'NONE',  ( 0.000000000000000000, 0.000000000000000000, 1.000000000000000000 ) ) ;
#5073 = DIRECTION ( 'NONE',  ( 0.000000000000000000, 1.000000000000000000, 0.000000000000000000 ) ) ;
#5074 = CARTESIAN_POINT ( 'NONE',  ( 140.3856359024541973, 94.90549801902425031, 23.00000000000000000 ) ) ;
#5075 = PLANE ( 'NONE',  #5873 ) ;
#5076 = DIRECTION ( 'NONE',  ( 0.000000000000000000, 0.000000000000000000, -1.000000000000000000 ) ) ;
#5077 = VERTEX_POINT ( 'NONE', #8623 ) ;
#5078 = VECTOR ( 'NONE', #4925, 1000.000000000000000 ) ;
#5079 = CIRCLE ( 'NONE', #6862, 0.5000000000000004441 ) ;
#5080 = EDGE_CURVE ( 'NONE', #12858, #13546, #1389, .T. ) ;
#5081 = ORIENTED_EDGE ( 'NONE', *, *, #10536, .F. ) ;
#5082 = ORIENTED_EDGE ( 'NONE', *, *, #12419, .T. ) ;
#5083 = LINE ( 'NONE', #9431, #9042 ) ;
#5084 = ORIENTED_EDGE ( 'NONE', *, *, #12372, .F. ) ;
#5085 = ORIENTED_EDGE ( 'NONE', *, *, #8157, .T. ) ;
#5086 = DIRECTION ( 'NONE',  ( 1.000000000000000000, 0.000000000000000000, 0.000000000000000000 ) ) ;
#5087 = CARTESIAN_POINT ( 'NONE',  ( 0.000000000000000000, 8.500000000000000000, 0.000000000000000000 ) ) ;
#5088 = AXIS2_PLACEMENT_3D ( 'NONE', #125, #1241, #4337 ) ;
#5089 =( NAMED_UNIT ( * ) SI_UNIT ( $, .STERADIAN. ) SOLID_ANGLE_UNIT ( ) );
#5090 = CIRCLE ( 'NONE', #9109, 5.000000000000000888 ) ;
#5091 = AXIS2_PLACEMENT_3D ( 'NONE', #8239, #12502, #2961 ) ;
#5092 = CARTESIAN_POINT ( 'NONE',  ( -24.37001676333060018, -4.028726038184999858, 63.45000000000000284 ) ) ;
#5093 = CIRCLE ( 'NONE', #5963, 3.000000000000002665 ) ;
#5094 = PLANE ( 'NONE',  #6419 ) ;
#5095 = CARTESIAN_POINT ( 'NONE',  ( -1.059188295049996231, 27.97290950744599769, 64.85000000000000853 ) ) ;
#5096 = EDGE_CURVE ( 'NONE', #12408, #11864, #6293, .T. ) ;
#5097 =( GEOMETRIC_REPRESENTATION_CONTEXT ( 3 ) GLOBAL_UNCERTAINTY_ASSIGNED_CONTEXT ( ( #6416 ) ) GLOBAL_UNIT_ASSIGNED_CONTEXT ( ( #4949, #11717, #48 ) ) REPRESENTATION_CONTEXT ( 'NONE', 'WORKASPACE' ) );
#5098 = CONICAL_SURFACE ( 'NONE', #11789, 4.250000000000000000, 0.7853981633974518317 ) ;
#5099 = VECTOR ( 'NONE', #8088, 1000.000000000000000 ) ;
#5100 = EDGE_LOOP ( 'NONE', ( #8306, #10393 ) ) ;
#5101 = VECTOR ( 'NONE', #13428, 1000.000000000000000 ) ;
#5102 = CARTESIAN_POINT ( 'NONE',  ( -14.74723118919472853, 30.12306837293317230, 59.53343286463421435 ) ) ;
#5103 = ORIENTED_EDGE ( 'NONE', *, *, #10027, .T. ) ;
#5104 = ORIENTED_EDGE ( 'NONE', *, *, #7120, .F. ) ;
#5105 = CARTESIAN_POINT ( 'NONE',  ( -24.47918829505000105, 10.97290950744599947, 64.85000000000000853 ) ) ;
#5106 = EDGE_CURVE ( 'NONE', #6726, #6571, #961, .T. ) ;
#5107 = DIRECTION ( 'NONE',  ( 0.000000000000000000, 0.000000000000000000, 1.000000000000000000 ) ) ;
#5108 = CARTESIAN_POINT ( 'NONE',  ( -1.059188295049996231, 27.97290950744599769, 64.85000000000000853 ) ) ;
#5109 = ORIENTED_EDGE ( 'NONE', *, *, #7436, .T. ) ;
#5110 = PLANE ( 'NONE',  #3314 ) ;
#5111 = CARTESIAN_POINT ( 'NONE',  ( -5.640422211807260666, -16.89844320975769776, 0.000000000000000000 ) ) ;
#5112 = CARTESIAN_POINT ( 'NONE',  ( -5.309188295050000228, 27.97290950744599769, 64.85000000000000853 ) ) ;
#5113 = DIRECTION ( 'NONE',  ( 1.000000000000000000, 0.000000000000000000, 0.000000000000000000 ) ) ;
#5114 = CARTESIAN_POINT ( 'NONE',  ( -18.05918829504999934, 10.97290950744599947, 12.50000000000000000 ) ) ;
#5115 = CARTESIAN_POINT ( 'NONE',  ( -5.631644894983189431, 10.97290950744599947, 17.25000000000000000 ) ) ;
#5116 = CIRCLE ( 'NONE', #12707, 0.9499999999999995115 ) ;
#5117 = ADVANCED_FACE ( 'NONE', ( #12760 ), #13725, .T. ) ;
#5118 = ORIENTED_EDGE ( 'NONE', *, *, #616, .T. ) ;
#5119 = ORIENTED_EDGE ( 'NONE', *, *, #11520, .T. ) ;
#5120 = EDGE_LOOP ( 'NONE', ( #3154, #1025, #1155, #5726 ) ) ;
#5121 = EDGE_CURVE ( 'NONE', #973, #12867, #13658, .T. ) ;
#5122 = VECTOR ( 'NONE', #2588, 1000.000000000000000 ) ;
#5123 = AXIS2_PLACEMENT_3D ( 'NONE', #1502, #329, #4586 ) ;
#5124 = DIRECTION ( 'NONE',  ( -1.000000000000000000, 0.000000000000000000, 0.000000000000000000 ) ) ;
#5125 = CARTESIAN_POINT ( 'NONE',  ( -18.05918829504999934, 10.97290950744599947, 61.86500000000000199 ) ) ;
#5126 = LINE ( 'NONE', #11483, #1395 ) ;
#5127 = CARTESIAN_POINT ( 'NONE',  ( 24.03999999999999915, 2.944050905150237001E-15, 7.000000000000000000 ) ) ;
#5128 = CARTESIAN_POINT ( 'NONE',  ( 100.2760581142613603, 115.9375248198690826, 20.00000000000000000 ) ) ;
#5129 = DIRECTION ( 'NONE',  ( 1.000000000000000000, 0.000000000000000000, -0.000000000000000000 ) ) ;
#5130 = VERTEX_POINT ( 'NONE', #7560 ) ;
#5131 = ORIENTED_EDGE ( 'NONE', *, *, #4571, .F. ) ;
#5132 = AXIS2_PLACEMENT_3D ( 'NONE', #5207, #2023, #12816 ) ;
#5133 = VECTOR ( 'NONE', #10139, 1000.000000000000000 ) ;
#5134 = TOROIDAL_SURFACE ( 'NONE', #1794, 23.29163056034262169, 0.7500000000000000000 ) ;
#5135 = CARTESIAN_POINT ( 'NONE',  ( -41.50918829505000218, 27.97290950744599769, 17.25000000000000000 ) ) ;
#5136 = CARTESIAN_POINT ( 'NONE',  ( -10.81426999815532852, 15.06602133594271820, 7.000000000000000000 ) ) ;
#5137 = VERTEX_POINT ( 'NONE', #8493 ) ;
#5138 = DIRECTION ( 'NONE',  ( 1.000000000000000000, 0.000000000000000000, 0.000000000000000000 ) ) ;
#5139 = CARTESIAN_POINT ( 'NONE',  ( -24.03999999999999915, 0.000000000000000000, 0.000000000000000000 ) ) ;
#5140 = CARTESIAN_POINT ( 'NONE',  ( 140.3856359024541973, 108.9054980190242503, 23.00000000000000000 ) ) ;
#5141 = AXIS2_PLACEMENT_3D ( 'NONE', #9913, #1509, #13247 ) ;
#5142 = AXIS2_PLACEMENT_3D ( 'NONE', #763, #824, #12500 ) ;
#5143 = CARTESIAN_POINT ( 'NONE',  ( 27.50000000000001066, 9.000000000000000000, -30.00000000000000355 ) ) ;
#5144 = ORIENTED_EDGE ( 'NONE', *, *, #2829, .F. ) ;
#5145 = CARTESIAN_POINT ( 'NONE',  ( -1.059188295049996231, 10.97290950744599947, 62.14999999999999858 ) ) ;
#5146 = VECTOR ( 'NONE', #8792, 1000.000000000000000 ) ;
#5147 = MANIFOLD_SOLID_BREP ( 'NONE', #12653 ) ;
#5148 = CARTESIAN_POINT ( 'NONE',  ( -18.05918829504999934, 10.97290950744599947, 62.14999999999999858 ) ) ;
#5149 = EDGE_CURVE ( 'NONE', #722, #13003, #6522, .T. ) ;
#5150 = CARTESIAN_POINT ( 'NONE',  ( -18.05918829504999934, 10.00028003023991907, 62.14999999999999858 ) ) ;
#5151 = DIRECTION ( 'NONE',  ( 0.000000000000000000, -0.000000000000000000, -1.000000000000000000 ) ) ;
#5152 = CARTESIAN_POINT ( 'NONE',  ( 44.88563590245420443, 104.1554980190242361, 23.00000000000000000 ) ) ;
#5153 = ORIENTED_EDGE ( 'NONE', *, *, #1161, .F. ) ;
#5154 = VERTEX_POINT ( 'NONE', #9833 ) ;
#5155 = CIRCLE ( 'NONE', #7356, 1.500000000000001332 ) ;
#5156 = SHAPE_REPRESENTATION ( 'Contact Pads', ( #6434 ), #2891 ) ;
#5157 = VECTOR ( 'NONE', #6450, 999.9999999999998863 ) ;
#5158 = AXIS2_PLACEMENT_3D ( 'NONE', #13793, #3014, #3966 ) ;
#5159 = ORIENTED_EDGE ( 'NONE', *, *, #88, .F. ) ;
#5160 = EDGE_CURVE ( 'NONE', #4325, #11902, #9435, .T. ) ;
#5161 = CARTESIAN_POINT ( 'NONE',  ( -35.05918829505000645, -6.027090492554000534, 0.000000000000000000 ) ) ;
#5162 = DIRECTION ( 'NONE',  ( 0.000000000000000000, 0.000000000000000000, 1.000000000000000000 ) ) ;
#5163 =( LENGTH_UNIT ( ) NAMED_UNIT ( * ) SI_UNIT ( .MILLI., .METRE. ) );
#5164 = EDGE_CURVE ( 'NONE', #12860, #13545, #505, .T. ) ;
#5165 = CARTESIAN_POINT ( 'NONE',  ( -18.05918829504999934, 2.872909508741170015, 63.35000000000700027 ) ) ;
#5166 = EDGE_CURVE ( 'NONE', #1998, #1301, #6597, .T. ) ;
#5167 = CIRCLE ( 'NONE', #13420, 6.000000000000000888 ) ;
#5168 = CARTESIAN_POINT ( 'NONE',  ( -41.50918829505000218, -6.027090492554000534, 5.250000000000000000 ) ) ;
#5169 = AXIS2_PLACEMENT_3D ( 'NONE', #5054, #13506, #4926 ) ;
#5170 = ORIENTED_EDGE ( 'NONE', *, *, #9124, .T. ) ;
#5171 = CARTESIAN_POINT ( 'NONE',  ( -14.48404530696549841, 30.08351321291744185, 55.79525418935277514 ) ) ;
#5172 = ORIENTED_EDGE ( 'NONE', *, *, #13461, .T. ) ;
#5173 = VERTEX_POINT ( 'NONE', #12128 ) ;
#5174 = ORIENTED_EDGE ( 'NONE', *, *, #7725, .T. ) ;
#5175 = CYLINDRICAL_SURFACE ( 'NONE', #8840, 6.450000000000019718 ) ;
#5176 = CARTESIAN_POINT ( 'NONE',  ( 44.63563590245420443, 108.9054980190242503, 20.00000000000000000 ) ) ;
#5177 = CARTESIAN_POINT ( 'NONE',  ( 42.63563590245419732, 111.0390816101113387, 20.00000000000000000 ) ) ;
#5178 = ORIENTED_EDGE ( 'NONE', *, *, #7879, .F. ) ;
#5179 = CARTESIAN_POINT ( 'NONE',  ( 6.940811704950004213, 32.97290950744599769, 10.00000000000000000 ) ) ;
#5180 = CYLINDRICAL_SURFACE ( 'NONE', #8668, 6.449999999999997513 ) ;
#5181 = EDGE_CURVE ( 'NONE', #8888, #2367, #12766, .T. ) ;
#5182 = CARTESIAN_POINT ( 'NONE',  ( -18.05918829504999934, 10.97290950744599947, 61.65955166399999854 ) ) ;
#5183 = LINE ( 'NONE', #9643, #9678 ) ;
#5184 = ADVANCED_FACE ( 'NONE', ( #3473 ), #11079, .T. ) ;
#5185 = CARTESIAN_POINT ( 'NONE',  ( -16.55945684168713683, 27.90662751739518654, 57.54990028585785922 ) ) ;
#5186 = EDGE_CURVE ( 'NONE', #13667, #11468, #13095, .T. ) ;
#5187 = CARTESIAN_POINT ( 'NONE',  ( -18.05918829504999934, 10.97290950744599947, 60.60999999999999943 ) ) ;
#5188 = EDGE_CURVE ( 'NONE', #10557, #4292, #11981, .T. ) ;
#5189 = EDGE_LOOP ( 'NONE', ( #6093, #9371 ) ) ;
#5190 = ORIENTED_EDGE ( 'NONE', *, *, #789, .T. ) ;
#5191 = EDGE_LOOP ( 'NONE', ( #3405, #4702, #10938, #7876 ) ) ;
#5192 = CARTESIAN_POINT ( 'NONE',  ( -10.38347696868452097, 26.08535324214045303, 58.35000000000000142 ) ) ;
#5193 = CARTESIAN_POINT ( 'NONE',  ( 42.63563590245419732, 87.03908161011138134, 19.68933982822018081 ) ) ;
#5194 = EDGE_CURVE ( 'NONE', #11380, #10426, #12331, .T. ) ;
#5195 = DIRECTION ( 'NONE',  ( -0.000000000000000000, 1.000000000000000000, -0.000000000000000000 ) ) ;
#5196 = CARTESIAN_POINT ( 'NONE',  ( -19.05204298599095480, 26.94232003179371304, 56.22521585200335181 ) ) ;
#5197 = DIRECTION ( 'NONE',  ( 1.000000000000000000, 0.000000000000000000, 0.000000000000000000 ) ) ;
#5198 = CARTESIAN_POINT ( 'NONE',  ( -1.059188295049996231, -6.027090492554000534, 68.85549045786049760 ) ) ;
#5199 = DIRECTION ( 'NONE',  ( 0.000000000000000000, 0.000000000000000000, 1.000000000000000000 ) ) ;
#5200 = SHAPE_DEFINITION_REPRESENTATION ( #5684, #13195 ) ;
#5201 = EDGE_CURVE ( 'NONE', #1818, #3446, #1496, .T. ) ;
#5202 = AXIS2_PLACEMENT_3D ( 'NONE', #13495, #3937, #644 ) ;
#5203 = EDGE_LOOP ( 'NONE', ( #11665, #6449, #13404, #6649 ) ) ;
#5204 = ORIENTED_EDGE ( 'NONE', *, *, #789, .F. ) ;
#5205 = CYLINDRICAL_SURFACE ( 'NONE', #792, 2.000000000000001776 ) ;
#5206 = ORIENTED_EDGE ( 'NONE', *, *, #9015, .T. ) ;
#5207 = CARTESIAN_POINT ( 'NONE',  ( -18.05918829504999934, 10.97290950744599947, 58.54999999999999716 ) ) ;
#5208 = PLANE ( 'NONE',  #13313 ) ;
#5209 = CARTESIAN_POINT ( 'NONE',  ( 140.6356359024541973, 113.0390816101113387, 19.25000000000000000 ) ) ;
#5210 = DIRECTION ( 'NONE',  ( 0.000000000000000000, 0.000000000000000000, 1.000000000000000000 ) ) ;
#5211 = CARTESIAN_POINT ( 'NONE',  ( 5.999999999999999112, -12.00000000000000178, 7.000000000000000000 ) ) ;
#5212 = MANIFOLD_SOLID_BREP ( 'NONE', #110 ) ;
#5213 = CARTESIAN_POINT ( 'NONE',  ( -1.059188295049996231, 27.97290950744599769, 7.250000000000000000 ) ) ;
#5214 = CARTESIAN_POINT ( 'NONE',  ( -18.05918829504999934, 10.97290950744599947, 30.59999999999999787 ) ) ;
#5215 = DIRECTION ( 'NONE',  ( 1.000000000000000000, 1.290957005378089519E-15, 0.000000000000000000 ) ) ;
#5216 = CARTESIAN_POINT ( 'NONE',  ( 42.63563590245419732, 111.0390816101113387, 19.25000000000000000 ) ) ;
#5217 = EDGE_CURVE ( 'NONE', #7297, #7051, #10873, .T. ) ;
#5218 = ORIENTED_EDGE ( 'NONE', *, *, #577, .F. ) ;
#5219 = VERTEX_POINT ( 'NONE', #1292 ) ;
#5220 = CARTESIAN_POINT ( 'NONE',  ( 140.6356359024541973, 94.90549801902425031, 22.75000000000000000 ) ) ;
#5221 = EDGE_LOOP ( 'NONE', ( #11359, #5159, #2907, #7001 ) ) ;
#5222 = ORIENTED_EDGE ( 'NONE', *, *, #5332, .T. ) ;
#5223 = DIRECTION ( 'NONE',  ( 0.000000000000000000, 1.000000000000000000, 0.000000000000000000 ) ) ;
#5224 = CARTESIAN_POINT ( 'NONE',  ( -10.82033510625394079, -2.574630058508199593, 62.14999999999999858 ) ) ;
#5225 = DIRECTION ( 'NONE',  ( 0.000000000000000000, 1.000000000000000000, 0.000000000000000000 ) ) ;
#5226 = LINE ( 'NONE', #2885, #13120 ) ;
#5227 = DIRECTION ( 'NONE',  ( 0.000000000000000000, 0.000000000000000000, 1.000000000000000000 ) ) ;
#5228 =( BOUNDED_CURVE ( )  B_SPLINE_CURVE ( 3, ( #9860, #6827, #4749, #4606 ),
 .UNSPECIFIED., .F., .F. ) 
 B_SPLINE_CURVE_WITH_KNOTS ( ( 4, 4 ),
 ( 0.000000000000000000, 1.570796326794896558 ),
 .UNSPECIFIED. ) 
 CURVE ( )  GEOMETRIC_REPRESENTATION_ITEM ( )  RATIONAL_B_SPLINE_CURVE ( ( 1.000000000000000000, 0.8047378541243649375, 0.8047378541243649375, 1.000000000000000000 ) ) 
 REPRESENTATION_ITEM ( '' )  );
#5229 = ADVANCED_FACE ( 'NONE', ( #8834 ), #257, .F. ) ;
#5230 = EDGE_CURVE ( 'NONE', #13004, #12299, #295, .T. ) ;
#5231 = ORIENTED_EDGE ( 'NONE', *, *, #4590, .F. ) ;
#5232 = ADVANCED_FACE ( 'NONE', ( #9192, #6947 ), #9044, .T. ) ;
#5233 = CARTESIAN_POINT ( 'NONE',  ( -14.76278877871134299, 30.12521254568601847, 55.14084190974008237 ) ) ;
#5234 = EDGE_LOOP ( 'NONE', ( #8977, #11823, #8325, #9265 ) ) ;
#5235 = ORIENTED_EDGE ( 'NONE', *, *, #9946, .T. ) ;
#5236 = LINE ( 'NONE', #13298, #9060 ) ;
#5237 = LINE ( 'NONE', #11735, #5026 ) ;
#5238 = DIRECTION ( 'NONE',  ( -1.000000000000000000, 0.000000000000000000, 0.000000000000000000 ) ) ;
#5239 = CARTESIAN_POINT ( 'NONE',  ( 4.599650328638321461, 8.500000000000001776, 9.878124499050784380 ) ) ;
#5240 = DIRECTION ( 'NONE',  ( -1.000000000000000000, 0.000000000000000000, 0.000000000000000000 ) ) ;
#5241 = DIRECTION ( 'NONE',  ( 3.441911658684139926E-17, 0.000000000000000000, 1.000000000000000000 ) ) ;
#5242 = LINE ( 'NONE', #9513, #4709 ) ;
#5243 = CIRCLE ( 'NONE', #6586, 9.999999999999994671 ) ;
#5244 = EDGE_CURVE ( 'NONE', #10600, #13687, #10554, .T. ) ;
#5245 = EDGE_CURVE ( 'NONE', #11588, #11467, #1169, .T. ) ;
#5246 = ORIENTED_EDGE ( 'NONE', *, *, #8102, .T. ) ;
#5247 = ORIENTED_EDGE ( 'NONE', *, *, #7641, .F. ) ;
#5248 = ORIENTED_EDGE ( 'NONE', *, *, #1348, .T. ) ;
#5249 = DIRECTION ( 'NONE',  ( 1.000000000000000000, 0.000000000000000000, 0.000000000000000000 ) ) ;
#5250 = DIRECTION ( 'NONE',  ( 0.000000000000000000, 0.000000000000000000, 1.000000000000000000 ) ) ;
#5251 = VERTEX_POINT ( 'NONE', #12399 ) ;
#5252 = CIRCLE ( 'NONE', #11068, 18.50000000000000000 ) ;
#5253 = CARTESIAN_POINT ( 'NONE',  ( -35.05918829505000645, -6.027090492554000534, 5.250000000000000000 ) ) ;
#5254 = EDGE_CURVE ( 'NONE', #5356, #10337, #13436, .T. ) ;
#5255 = DIRECTION ( 'NONE',  ( 0.000000000000000000, 0.000000000000000000, 1.000000000000000000 ) ) ;
#5256 = CARTESIAN_POINT ( 'NONE',  ( -18.05918829504999934, 10.97290950744599947, 14.00000000000000000 ) ) ;
#5257 = CARTESIAN_POINT ( 'NONE',  ( -5.631644894983189431, 10.97290950744599947, 5.250000000000000000 ) ) ;
#5258 = DIRECTION ( 'NONE',  ( 0.000000000000000000, -0.000000000000000000, -1.000000000000000000 ) ) ;
#5259 = CONTEXT_DEPENDENT_SHAPE_REPRESENTATION ( #6621, #3594 ) ;
#5260 = ORIENTED_EDGE ( 'NONE', *, *, #7142, .F. ) ;
#5261 = EDGE_CURVE ( 'NONE', #95, #1822, #8090, .T. ) ;
#5262 = AXIS2_PLACEMENT_3D ( 'NONE', #11464, #2710, #588 ) ;
#5263 = ORIENTED_EDGE ( 'NONE', *, *, #7719, .F. ) ;
#5264 = LINE ( 'NONE', #7417, #13739 ) ;
#5265 = FACE_BOUND ( 'NONE', #11806, .T. ) ;
#5266 = DIRECTION ( 'NONE',  ( 0.000000000000000000, 0.000000000000000000, -1.000000000000000000 ) ) ;
#5267 = CARTESIAN_POINT ( 'NONE',  ( -18.05918829504999934, 10.97290950744599947, 56.84999999999999432 ) ) ;
#5268 = EDGE_CURVE ( 'NONE', #4170, #6531, #13370, .T. ) ;
#5269 = DIRECTION ( 'NONE',  ( 0.000000000000000000, 0.000000000000000000, 1.000000000000000000 ) ) ;
#5270 = SURFACE_STYLE_USAGE ( .BOTH. , #10591 ) ;
#5271 = DIRECTION ( 'NONE',  ( 0.000000000000000000, 0.000000000000000000, -1.000000000000000000 ) ) ;
#5272 = CARTESIAN_POINT ( 'NONE',  ( -18.05918829504999934, 7.130333642789880244, 17.25000000000000000 ) ) ;
#5273 = CARTESIAN_POINT ( 'NONE',  ( 1.940811704950003991, 27.97290950744599769, 0.000000000000000000 ) ) ;
#5274 = PRESENTATION_LAYER_ASSIGNMENT (  '', '', ( #812 ) ) ;
#5275 = FACE_OUTER_BOUND ( 'NONE', #13225, .T. ) ;
#5276 =( NAMED_UNIT ( * ) SI_UNIT ( $, .STERADIAN. ) SOLID_ANGLE_UNIT ( ) );
#5277 = EDGE_CURVE ( 'NONE', #9433, #7877, #11224, .T. ) ;
#5278 = ORIENTED_EDGE ( 'NONE', *, *, #10317, .T. ) ;
#5279 = ORIENTED_EDGE ( 'NONE', *, *, #6877, .F. ) ;
#5280 = AXIS2_PLACEMENT_3D ( 'NONE', #1654, #9131, #12204 ) ;
#5281 = CARTESIAN_POINT ( 'NONE',  ( -7.640422211807256225, -16.89844320975769776, 0.000000000000000000 ) ) ;
#5282 = ORIENTED_EDGE ( 'NONE', *, *, #3726, .T. ) ;
#5283 = VERTEX_POINT ( 'NONE', #13302 ) ;
#5284 = ORIENTED_EDGE ( 'NONE', *, *, #6306, .T. ) ;
#5285 = ORIENTED_EDGE ( 'NONE', *, *, #9968, .F. ) ;
#5286 = CARTESIAN_POINT ( 'NONE',  ( -13.44794508215399453, 8.373466233319598828, 68.55654520525476414 ) ) ;
#5287 = EDGE_CURVE ( 'NONE', #9802, #7749, #2083, .T. ) ;
#5288 = LINE ( 'NONE', #11453, #8034 ) ;
#5289 = FACE_BOUND ( 'NONE', #6849, .T. ) ;
#5290 = CARTESIAN_POINT ( 'NONE',  ( -3.999999999999998224, -1.301042606982605321E-15, -65.00000000000000000 ) ) ;
#5291 = DIRECTION ( 'NONE',  ( 0.7071067811865451302, -0.7071067811865500152, -0.000000000000000000 ) ) ;
#5292 = AXIS2_PLACEMENT_3D ( 'NONE', #10309, #5053, #10370 ) ;
#5293 = CONICAL_SURFACE ( 'NONE', #6448, 17.00000000000000000, 0.7853981633974476129 ) ;
#5294 = AXIS2_PLACEMENT_3D ( 'NONE', #1364, #2715, #10106 ) ;
#5295 = VERTEX_POINT ( 'NONE', #5824 ) ;
#5296 = LINE ( 'NONE', #67, #346 ) ;
#5297 = AXIS2_PLACEMENT_3D ( 'NONE', #4398, #10825, #2175 ) ;
#5298 = EDGE_LOOP ( 'NONE', ( #10558, #13361, #13222, #9460 ) ) ;
#5299 = AXIS2_PLACEMENT_3D ( 'NONE', #5840, #11032, #2660 ) ;
#5300 = VECTOR ( 'NONE', #7585, 1000.000000000000114 ) ;
#5301 = ORIENTED_EDGE ( 'NONE', *, *, #6271, .T. ) ;
#5302 = CARTESIAN_POINT ( 'NONE',  ( -3.999999999999998224, -1.301042606982605321E-15, -65.00000000000000000 ) ) ;
#5303 = CIRCLE ( 'NONE', #170, 6.049999999999999822 ) ;
#5304 = CARTESIAN_POINT ( 'NONE',  ( 4.599650328638321461, 8.500000000000000000, 5.878124499050807472 ) ) ;
#5305 = CYLINDRICAL_SURFACE ( 'NONE', #10518, 2.500000000000000000 ) ;
#5306 = CARTESIAN_POINT ( 'NONE',  ( 4.599650328638321461, 0.000000000000000000, 7.878124499050794149 ) ) ;
#5307 = CARTESIAN_POINT ( 'NONE',  ( 75.58559257550551536, 82.08927268643400055, 0.7500000000000006661 ) ) ;
#5308 = ADVANCED_FACE ( 'NONE', ( #12341 ), #8198, .F. ) ;
#5309 = FACE_OUTER_BOUND ( 'NONE', #11026, .T. ) ;
#5310 =( GEOMETRIC_REPRESENTATION_CONTEXT ( 3 ) GLOBAL_UNCERTAINTY_ASSIGNED_CONTEXT ( ( #12986 ) ) GLOBAL_UNIT_ASSIGNED_CONTEXT ( ( #2098, #9840, #5477 ) ) REPRESENTATION_CONTEXT ( 'NONE', 'WORKASPACE' ) );
#5311 = CIRCLE ( 'NONE', #10019, 17.00000000000000355 ) ;
#5312 = AXIS2_PLACEMENT_3D ( 'NONE', #7225, #5073, #8297 ) ;
#5313 = AXIS2_PLACEMENT_3D ( 'NONE', #2268, #5439, #8528 ) ;
#5314 = ORIENTED_EDGE ( 'NONE', *, *, #11858, .T. ) ;
#5315 = CARTESIAN_POINT ( 'NONE',  ( -12.69835982676941910, -4.028726038184999858, 62.14999999999999858 ) ) ;
#5316 = ORIENTED_EDGE ( 'NONE', *, *, #13055, .T. ) ;
#5317 = ORIENTED_EDGE ( 'NONE', *, *, #10146, .F. ) ;
#5318 = TOROIDAL_SURFACE ( 'NONE', #3993, 16.99999999999999645, 1.500000000000000000 ) ;
#5319 = DIRECTION ( 'NONE',  ( 0.000000000000000000, 0.000000000000000000, -1.000000000000000000 ) ) ;
#5320 = LINE ( 'NONE', #10714, #1979 ) ;
#5321 = VECTOR ( 'NONE', #6748, 1000.000000000000000 ) ;
#5322 = ORIENTED_EDGE ( 'NONE', *, *, #12335, .F. ) ;
#5323 = DIRECTION ( 'NONE',  ( 1.000000000000000000, -9.130123557772668088E-16, 0.000000000000000000 ) ) ;
#5324 = DIRECTION ( 'NONE',  ( 0.000000000000000000, 0.000000000000000000, 1.000000000000000000 ) ) ;
#5325 = FACE_OUTER_BOUND ( 'NONE', #7219, .T. ) ;
#5326 = CARTESIAN_POINT ( 'NONE',  ( 2.262399129208275017, -0.4981161769137599782, 5.250000000000000000 ) ) ;
#5327 = EDGE_CURVE ( 'NONE', #8057, #506, #10245, .T. ) ;
#5328 = CARTESIAN_POINT ( 'NONE',  ( 0.000000000000000000, -17.50000000000000000, 0.000000000000000000 ) ) ;
#5329 = EDGE_LOOP ( 'NONE', ( #7829, #836, #7966, #761 ) ) ;
#5330 = CIRCLE ( 'NONE', #6676, 16.75000000000000355 ) ;
#5331 = AXIS2_PLACEMENT_3D ( 'NONE', #5476, #4453, #3212 ) ;
#5332 = EDGE_CURVE ( 'NONE', #13079, #1264, #56, .T. ) ;
#5333 = DIRECTION ( 'NONE',  ( 0.4528443260392608360, 0.8915896008669278450, 0.000000000000000000 ) ) ;
#5334 = ORIENTED_EDGE ( 'NONE', *, *, #1432, .F. ) ;
#5335 = CARTESIAN_POINT ( 'NONE',  ( -40.05918829504999934, -11.02709049255400053, 10.00000000000000000 ) ) ;
#5336 = CARTESIAN_POINT ( 'NONE',  ( -24.20502162805000168, 10.97290950744599947, 61.10999999999999943 ) ) ;
#5337 = CARTESIAN_POINT ( 'NONE',  ( -18.05918829504999934, 10.97290950744599947, 60.04999999999999716 ) ) ;
#5338 = CARTESIAN_POINT ( 'NONE',  ( -20.81153244793331325, 30.19664696409543581, 54.32892173082856857 ) ) ;
#5339 = FILL_AREA_STYLE ('',( #2091 ) ) ;
#5340 = ORIENTED_EDGE ( 'NONE', *, *, #4604, .T. ) ;
#5341 = DIRECTION ( 'NONE',  ( -0.9496839325805421783, 0.3132098788326385663, 0.000000000000000000 ) ) ;
#5342 = CARTESIAN_POINT ( 'NONE',  ( -18.05918829504999934, 10.97290950744599947, 14.00000000000000000 ) ) ;
#5343 = DIRECTION ( 'NONE',  ( 0.000000000000000000, 0.000000000000000000, -1.000000000000000000 ) ) ;
#5344 = EDGE_CURVE ( 'NONE', #3017, #10572, #2717, .T. ) ;
#5345 = ORIENTED_EDGE ( 'NONE', *, *, #12034, .F. ) ;
#5346 = CARTESIAN_POINT ( 'NONE',  ( -27.61808667955315144, -3.085093966544995236, 62.14999999999999858 ) ) ;
#5347 = CONICAL_SURFACE ( 'NONE', #1333, 7.618085573000000110, 0.1329427246665018103 ) ;
#5348 = CIRCLE ( 'NONE', #3360, 4.750000000000000888 ) ;
#5349 = EDGE_CURVE ( 'NONE', #6678, #918, #5629, .T. ) ;
#5350 = EDGE_CURVE ( 'NONE', #9587, #10693, #656, .T. ) ;
#5351 = AXIS2_PLACEMENT_3D ( 'NONE', #12064, #4593, #8846 ) ;
#5352 = CARTESIAN_POINT ( 'NONE',  ( -35.05918829505000645, -6.027090492554000534, 64.85000000000000853 ) ) ;
#5353 = VECTOR ( 'NONE', #13137, 1000.000000000000114 ) ;
#5354 = VECTOR ( 'NONE', #9213, 1000.000000000000000 ) ;
#5355 = ORIENTED_EDGE ( 'NONE', *, *, #5186, .T. ) ;
#5356 = VERTEX_POINT ( 'NONE', #11143 ) ;
#5357 = ORIENTED_EDGE ( 'NONE', *, *, #3001, .T. ) ;
#5358 = DIRECTION ( 'NONE',  ( 0.1325514707600310149, 0.000000000000000000, -0.9911761234005551646 ) ) ;
#5359 = PLANE ( 'NONE',  #12063 ) ;
#5360 = CARTESIAN_POINT ( 'NONE',  ( -40.05918829504999934, -11.02709049255400053, 10.00000000000000000 ) ) ;
#5361 = ADVANCED_FACE ( 'NONE', ( #4924 ), #5951, .T. ) ;
#5362 = DIRECTION ( 'NONE',  ( 0.000000000000000000, 0.000000000000000000, 1.000000000000000000 ) ) ;
#5363 = AXIS2_PLACEMENT_3D ( 'NONE', #10729, #1150, #7281 ) ;
#5364 = VECTOR ( 'NONE', #12574, 1000.000000000000000 ) ;
#5365 = AXIS2_PLACEMENT_3D ( 'NONE', #11221, #6808, #1574 ) ;
#5366 = ADVANCED_FACE ( 'NONE', ( #1571 ), #10110, .F. ) ;
#5367 = VERTEX_POINT ( 'NONE', #1922 ) ;
#5368 = DIRECTION ( 'NONE',  ( 0.000000000000000000, 0.000000000000000000, 1.000000000000000000 ) ) ;
#5369 = ORIENTED_EDGE ( 'NONE', *, *, #11211, .F. ) ;
#5370 = CARTESIAN_POINT ( 'NONE',  ( -6.000000000000000888, 11.99999999999999822, 0.000000000000000000 ) ) ;
#5371 = CIRCLE ( 'NONE', #5590, 6.000000000000000888 ) ;
#5372 = DIRECTION ( 'NONE',  ( 0.000000000000000000, 0.000000000000000000, 1.000000000000000000 ) ) ;
#5373 = CIRCLE ( 'NONE', #3382, 17.00000000000000355 ) ;
#5374 = SURFACE_STYLE_USAGE ( .BOTH. , #6427 ) ;
#5375 = AXIS2_PLACEMENT_3D ( 'NONE', #13098, #2514, #3546 ) ;
#5376 = CARTESIAN_POINT ( 'NONE',  ( -10.38347696868452097, 26.08535324214045303, 57.54999999999999716 ) ) ;
#5377 = PLANE ( 'NONE',  #6655 ) ;
#5378 = DIRECTION ( 'NONE',  ( 1.000000000000000000, 0.000000000000000000, 0.000000000000000000 ) ) ;
#5379 = DIRECTION ( 'NONE',  ( -1.000000000000000000, 0.000000000000000000, 0.000000000000000000 ) ) ;
#5380 = EDGE_CURVE ( 'NONE', #3998, #9144, #9659, .T. ) ;
#5381 = STYLED_ITEM ( 'NONE', ( #5994 ), #4577 ) ;
#5382 = EDGE_CURVE ( 'NONE', #7248, #6726, #5126, .T. ) ;
#5383 = ORIENTED_EDGE ( 'NONE', *, *, #88, .T. ) ;
#5384 = ORIENTED_EDGE ( 'NONE', *, *, #11656, .F. ) ;
#5385 = LINE ( 'NONE', #3249, #2819 ) ;
#5386 = ORIENTED_EDGE ( 'NONE', *, *, #12966, .T. ) ;
#5387 = VERTEX_POINT ( 'NONE', #9598 ) ;
#5388 = ORIENTED_EDGE ( 'NONE', *, *, #5766, .F. ) ;
#5389 = DIRECTION ( 'NONE',  ( 1.000000000000000000, -0.000000000000000000, -0.000000000000000000 ) ) ;
#5390 = CYLINDRICAL_SURFACE ( 'NONE', #11780, 0.7500000000000000000 ) ;
#5391 = EDGE_LOOP ( 'NONE', ( #13555, #9828, #5064, #1886 ) ) ;
#5392 = DIRECTION ( 'NONE',  ( -0.3202092937642119774, -0.6304490528084089052, 0.7071067811865507924 ) ) ;
#5393 = CARTESIAN_POINT ( 'NONE',  ( -18.05918829504999934, 10.97290950744599947, 61.25000000000000000 ) ) ;
#5394 = DIRECTION ( 'NONE',  ( 0.000000000000000000, -1.000000000000000000, 0.000000000000000000 ) ) ;
#5395 = DIRECTION ( 'NONE',  ( 0.000000000000000000, 0.000000000000000000, -1.000000000000000000 ) ) ;
#5396 = DIRECTION ( 'NONE',  ( 0.000000000000000000, 0.000000000000000000, -1.000000000000000000 ) ) ;
#5397 = ITEM_DEFINED_TRANSFORMATION ( 'NONE', 'NONE', #5770,  #6434 ) ;
#5398 = ADVANCED_BREP_SHAPE_REPRESENTATION ( '', ( #9635, #6434 ), #5310 ) ;
#5399 = CIRCLE ( 'NONE', #3201, 24.03999999999999915 ) ;
#5400 = PRODUCT ( 'Gripper Arm', 'Gripper Arm', '', ( #9120 ) ) ;
#5401 = ADVANCED_FACE ( 'NONE', ( #28 ), #1137, .T. ) ;
#5402 = ORIENTED_EDGE ( 'NONE', *, *, #7719, .T. ) ;
#5403 = ORIENTED_EDGE ( 'NONE', *, *, #998, .F. ) ;
#5404 = EDGE_CURVE ( 'NONE', #11879, #1026, #6451, .T. ) ;
#5405 = LINE ( 'NONE', #6331, #3054 ) ;
#5406 = CARTESIAN_POINT ( 'NONE',  ( -3.999999999999997335, 2.000000000000000000, 0.000000000000000000 ) ) ;
#5407 = EDGE_CURVE ( 'NONE', #9458, #7458, #5399, .T. ) ;
#5408 = CARTESIAN_POINT ( 'NONE',  ( 16.08092853089229024, 4.500000000000000000, -9.237812082545193704 ) ) ;
#5409 = FACE_OUTER_BOUND ( 'NONE', #10244, .T. ) ;
#5410 = CARTESIAN_POINT ( 'NONE',  ( -20.23067423319998426, 30.25856101892194872, 53.76667154643602231 ) ) ;
#5411 = EDGE_LOOP ( 'NONE', ( #9740, #6725, #379, #6459 ) ) ;
#5412 = CARTESIAN_POINT ( 'NONE',  ( 7.500000000000000000, -0.5000000000000017764, -65.00000000000000000 ) ) ;
#5413 = CARTESIAN_POINT ( 'NONE',  ( -19.91165729514404603, 13.07251866242952154, 23.90000000000000213 ) ) ;
#5414 = DIRECTION ( 'NONE',  ( 0.000000000000000000, 0.000000000000000000, -1.000000000000000000 ) ) ;
#5415 = CIRCLE ( 'NONE', #9893, 1.999999999999995781 ) ;
#5416 = CARTESIAN_POINT ( 'NONE',  ( -12.54628844161313950, -7.366404416634599883, 62.14999999999999858 ) ) ;
#5417 = EDGE_CURVE ( 'NONE', #8947, #3062, #8764, .T. ) ;
#5418 = EDGE_CURVE ( 'NONE', #11380, #11449, #9400, .T. ) ;
#5419 = ORIENTED_EDGE ( 'NONE', *, *, #5080, .T. ) ;
#5420 = AXIS2_PLACEMENT_3D ( 'NONE', #4682, #7941, #4543 ) ;
#5421 = FACE_BOUND ( 'NONE', #13491, .T. ) ;
#5422 = ORIENTED_EDGE ( 'NONE', *, *, #12998, .F. ) ;
#5423 = ORIENTED_EDGE ( 'NONE', *, *, #13232, .T. ) ;
#5424 = ORIENTED_EDGE ( 'NONE', *, *, #13194, .T. ) ;
#5425 = CYLINDRICAL_SURFACE ( 'NONE', #388, 4.750000000000000888 ) ;
#5426 = ADVANCED_FACE ( 'NONE', ( #12745 ), #7209, .F. ) ;
#5427 = LINE ( 'NONE', #10679, #12947 ) ;
#5428 = DIRECTION ( 'NONE',  ( 1.000000000000000000, 0.000000000000000000, -0.000000000000000000 ) ) ;
#5429 = DIRECTION ( 'NONE',  ( -0.000000000000000000, -0.000000000000000000, 1.000000000000000000 ) ) ;
#5430 = ADVANCED_FACE ( 'NONE', ( #867 ), #3197, .F. ) ;
#5431 = DIRECTION ( 'NONE',  ( 1.000000000000000000, 0.000000000000000000, 0.000000000000000000 ) ) ;
#5432 = DIRECTION ( 'NONE',  ( 0.000000000000000000, 0.000000000000000000, -1.000000000000000000 ) ) ;
#5433 = ORIENTED_EDGE ( 'NONE', *, *, #9877, .F. ) ;
#5434 = ADVANCED_FACE ( 'NONE', ( #2210 ), #10514, .T. ) ;
#5435 = CARTESIAN_POINT ( 'NONE',  ( -15.95913914146609613, 30.26546654951570048, 53.70790935732234317 ) ) ;
#5436 = EDGE_LOOP ( 'NONE', ( #3049, #4057, #222, #5936, #9695, #938, #11323, #3136 ) ) ;
#5437 = FACE_OUTER_BOUND ( 'NONE', #6074, .T. ) ;
#5438 = CARTESIAN_POINT ( 'NONE',  ( -21.16117192841894834, 4.865520741507539881, 64.54999999999999716 ) ) ;
#5439 = DIRECTION ( 'NONE',  ( 0.000000000000000000, 0.000000000000000000, 1.000000000000000000 ) ) ;
#5440 = EDGE_CURVE ( 'NONE', #8353, #5838, #8773, .T. ) ;
#5441 = CARTESIAN_POINT ( 'NONE',  ( 140.3856359024541973, 0.000000000000000000, 22.75000000000000000 ) ) ;
#5442 = DIRECTION ( 'NONE',  ( 0.000000000000000000, 0.000000000000000000, -1.000000000000000000 ) ) ;
#5443 = ORIENTED_EDGE ( 'NONE', *, *, #4248, .T. ) ;
#5444 = EDGE_CURVE ( 'NONE', #9493, #1604, #12041, .T. ) ;
#5445 = VECTOR ( 'NONE', #1614, 1000.000000000000000 ) ;
#5446 = LINE ( 'NONE', #2416, #8810 ) ;
#5447 = APPLICATION_CONTEXT ( 'automotive_design' ) ;
#5448 = ORIENTED_EDGE ( 'NONE', *, *, #6412, .F. ) ;
#5449 = EDGE_LOOP ( 'NONE', ( #11527, #8507, #9407, #3588 ) ) ;
#5450 = EDGE_LOOP ( 'NONE', ( #6834, #6405, #5673, #11515 ) ) ;
#5451 = CARTESIAN_POINT ( 'NONE',  ( -27.15409092487699994, 0.3335619008453594714, 63.45000000000000284 ) ) ;
#5452 = DIRECTION ( 'NONE',  ( -1.000000000000000000, 0.000000000000000000, 0.000000000000000000 ) ) ;
#5453 = ORIENTED_EDGE ( 'NONE', *, *, #2288, .T. ) ;
#5454 = ADVANCED_FACE ( 'NONE', ( #444 ), #5456, .T. ) ;
#5455 = CARTESIAN_POINT ( 'NONE',  ( -23.24102627739274851, -6.265087914666289670, 63.45000000000000284 ) ) ;
#5456 = CYLINDRICAL_SURFACE ( 'NONE', #6528, 34.70000000000000284 ) ;
#5457 = CYLINDRICAL_SURFACE ( 'NONE', #4414, 0.7500000000000000000 ) ;
#5458 = DIRECTION ( 'NONE',  ( 0.000000000000000000, 0.000000000000000000, -1.000000000000000000 ) ) ;
#5459 = CIRCLE ( 'NONE', #1226, 3.000000000000001332 ) ;
#5460 = DIRECTION ( 'NONE',  ( 1.000000000000000000, 0.000000000000000000, 0.000000000000000000 ) ) ;
#5461 = ORIENTED_EDGE ( 'NONE', *, *, #3088, .T. ) ;
#5462 = CONICAL_SURFACE ( 'NONE', #8154, 5.500000000000002665, 0.7853981633974433940 ) ;
#5463 = ORIENTED_EDGE ( 'NONE', *, *, #1868, .F. ) ;
#5464 = ORIENTED_EDGE ( 'NONE', *, *, #8408, .T. ) ;
#5465 = CIRCLE ( 'NONE', #2840, 10.74999999999999645 ) ;
#5466 = DIRECTION ( 'NONE',  ( -0.7050191076322684935, -0.7091883091770476710, -0.000000000000000000 ) ) ;
#5467 = DIRECTION ( 'NONE',  ( 1.000000000000000000, 0.000000000000000000, 0.000000000000000000 ) ) ;
#5468 = VERTEX_POINT ( 'NONE', #8971 ) ;
#5469 = DIRECTION ( 'NONE',  ( 0.000000000000000000, 0.000000000000000000, 1.000000000000000000 ) ) ;
#5470 = CARTESIAN_POINT ( 'NONE',  ( -19.35500534946005402, 30.32416700404740340, 53.25030877638827320 ) ) ;
#5471 = DIRECTION ( 'NONE',  ( 0.000000000000000000, 0.000000000000000000, 1.000000000000000000 ) ) ;
#5472 = ORIENTED_EDGE ( 'NONE', *, *, #5025, .F. ) ;
#5473 = DIRECTION ( 'NONE',  ( 0.000000000000000000, 0.000000000000000000, -1.000000000000000000 ) ) ;
#5474 = DIRECTION ( 'NONE',  ( -0.4678190685372678459, 0.5302313826179257950, 0.7071067811865516806 ) ) ;
#5475 = CARTESIAN_POINT ( 'NONE',  ( -18.05918829504999934, 10.97290950744599947, 62.14999999999999858 ) ) ;
#5476 = CARTESIAN_POINT ( 'NONE',  ( -5.631644894983189431, 10.97290950744599947, 5.250000000000000000 ) ) ;
#5477 =( NAMED_UNIT ( * ) SI_UNIT ( $, .STERADIAN. ) SOLID_ANGLE_UNIT ( ) );
#5478 = EDGE_CURVE ( 'NONE', #9008, #9150, #1272, .T. ) ;
#5479 = ORIENTED_EDGE ( 'NONE', *, *, #11052, .F. ) ;
#5480 = ORIENTED_EDGE ( 'NONE', *, *, #5812, .T. ) ;
#5481 = PLANE ( 'NONE',  #9949 ) ;
#5482 = ORIENTED_EDGE ( 'NONE', *, *, #6022, .T. ) ;
#5483 = VERTEX_POINT ( 'NONE', #11006 ) ;
#5484 = LINE ( 'NONE', #10816, #7137 ) ;
#5485 = DIRECTION ( 'NONE',  ( 0.000000000000000000, 0.000000000000000000, -1.000000000000000000 ) ) ;
#5486 = AXIS2_PLACEMENT_3D ( 'NONE', #1890, #3025, #5086 ) ;
#5487 = LINE ( 'NONE', #4538, #683 ) ;
#5488 = ORIENTED_EDGE ( 'NONE', *, *, #111, .F. ) ;
#5489 =( LENGTH_UNIT ( ) NAMED_UNIT ( * ) SI_UNIT ( .MILLI., .METRE. ) );
#5490 = CARTESIAN_POINT ( 'NONE',  ( 43.16596598834411225, 87.56941169600128205, 0.000000000000000000 ) ) ;
#5491 = DIRECTION ( 'NONE',  ( 1.000000000000000000, 0.000000000000000000, 0.000000000000000000 ) ) ;
#5492 = DIRECTION ( 'NONE',  ( -1.000000000000000000, 0.000000000000000000, 0.000000000000000000 ) ) ;
#5493 = CARTESIAN_POINT ( 'NONE',  ( 103.4499059006094512, 83.97306027416853169, 10.00000000000000000 ) ) ;
#5494 = ADVANCED_FACE ( 'NONE', ( #9735 ), #2496, .F. ) ;
#5495 = VECTOR ( 'NONE', #4375, 1000.000000000000000 ) ;
#5496 = CIRCLE ( 'NONE', #11104, 6.850000000000002309 ) ;
#5497 = EDGE_CURVE ( 'NONE', #10778, #525, #1422, .T. ) ;
#5498 = EDGE_CURVE ( 'NONE', #6848, #859, #7542, .T. ) ;
#5499 = CARTESIAN_POINT ( 'NONE',  ( -15.45975122988422257, 30.21441468582782974, 54.15812869781769479 ) ) ;
#5500 = ORIENTED_EDGE ( 'NONE', *, *, #10564, .T. ) ;
#5501 = FILL_AREA_STYLE_COLOUR ( '', #3724 ) ;
#5502 = SHAPE_REPRESENTATION ( 'Gripper Arm', ( #6434 ), #1075 ) ;
#5503 = CARTESIAN_POINT ( 'NONE',  ( -11.74835982676941981, -4.028726038184999858, 62.14999999999999858 ) ) ;
#5504 = VECTOR ( 'NONE', #5681, 1000.000000000000000 ) ;
#5505 = LINE ( 'NONE', #7445, #9629 ) ;
#5506 = EDGE_LOOP ( 'NONE', ( #1637, #6282, #3221, #7386, #9234 ) ) ;
#5507 = LINE ( 'NONE', #12918, #11563 ) ;
#5508 = CIRCLE ( 'NONE', #13323, 2.000000000000001776 ) ;
#5509 = DIRECTION ( 'NONE',  ( 0.000000000000000000, 0.000000000000000000, 1.000000000000000000 ) ) ;
#5510 = EDGE_CURVE ( 'NONE', #6605, #172, #6761, .T. ) ;
#5511 = DIRECTION ( 'NONE',  ( 0.000000000000000000, 1.000000000000000000, 0.000000000000000000 ) ) ;
#5512 = VECTOR ( 'NONE', #11385, 1000.000000000000000 ) ;
#5513 = VECTOR ( 'NONE', #6614, 1000.000000000000000 ) ;
#5514 = ORIENTED_EDGE ( 'NONE', *, *, #10939, .T. ) ;
#5515 = EDGE_LOOP ( 'NONE', ( #7881, #5464, #7910, #11430 ) ) ;
#5516 = EDGE_CURVE ( 'NONE', #11194, #13765, #6583, .T. ) ;
#5517 = VERTEX_POINT ( 'NONE', #12941 ) ;
#5518 = DIRECTION ( 'NONE',  ( 0.000000000000000000, 0.000000000000000000, -1.000000000000000000 ) ) ;
#5519 = ORIENTED_EDGE ( 'NONE', *, *, #8850, .T. ) ;
#5520 = VERTEX_POINT ( 'NONE', #3603 ) ;
#5521 = ORIENTED_EDGE ( 'NONE', *, *, #7031, .F. ) ;
#5522 = LINE ( 'NONE', #3387, #418 ) ;
#5523 = DIRECTION ( 'NONE',  ( 1.000000000000000000, 0.000000000000000000, 0.000000000000000000 ) ) ;
#5524 = ORIENTED_EDGE ( 'NONE', *, *, #13395, .F. ) ;
#5525 = LINE ( 'NONE', #6521, #10519 ) ;
#5526 = AXIS2_PLACEMENT_3D ( 'NONE', #2032, #9487, #13526 ) ;
#5527 = DIRECTION ( 'NONE',  ( 0.000000000000000000, 0.000000000000000000, 1.000000000000000000 ) ) ;
#5528 = CIRCLE ( 'NONE', #8895, 17.00000000000000355 ) ;
#5529 = DIRECTION ( 'NONE',  ( 0.000000000000000000, 0.000000000000000000, 1.000000000000000000 ) ) ;
#5530 = AXIS2_PLACEMENT_3D ( 'NONE', #7870, #8791, #6962 ) ;
#5531 = CARTESIAN_POINT ( 'NONE',  ( 92.63563590245421153, 99.03908161011133870, 0.000000000000000000 ) ) ;
#5532 = EDGE_CURVE ( 'NONE', #8353, #6343, #13233, .T. ) ;
#5533 = VECTOR ( 'NONE', #3370, 1000.000000000000000 ) ;
#5534 = DIRECTION ( 'NONE',  ( 0.000000000000000000, 0.000000000000000000, -1.000000000000000000 ) ) ;
#5535 = VERTEX_POINT ( 'NONE', #12114 ) ;
#5536 = EDGE_CURVE ( 'NONE', #8537, #12924, #10783, .T. ) ;
#5537 = ORIENTED_EDGE ( 'NONE', *, *, #4424, .T. ) ;
#5538 = AXIS2_PLACEMENT_3D ( 'NONE', #1893, #827, #6131 ) ;
#5539 = CIRCLE ( 'NONE', #10684, 9.999999999999994671 ) ;
#5540 = AXIS2_PLACEMENT_3D ( 'NONE', #5700, #12286, #9981 ) ;
#5541 = DIRECTION ( 'NONE',  ( 0.000000000000000000, 1.000000000000000000, 0.000000000000000000 ) ) ;
#5542 = EDGE_LOOP ( 'NONE', ( #9263, #6785, #13021, #1252 ) ) ;
#5543 = CARTESIAN_POINT ( 'NONE',  ( 92.63563590245421153, 99.03908161011133870, 19.25000000000000000 ) ) ;
#5544 = DIRECTION ( 'NONE',  ( 1.000000000000000000, 0.000000000000000000, -0.000000000000000000 ) ) ;
#5545 = DIRECTION ( 'NONE',  ( -1.000000000000000000, 0.000000000000000000, 0.000000000000000000 ) ) ;
#5546 = DIRECTION ( 'NONE',  ( 1.000000000000000000, 0.000000000000000000, 0.000000000000000000 ) ) ;
#5547 = ORIENTED_EDGE ( 'NONE', *, *, #10218, .T. ) ;
#5548 = CARTESIAN_POINT ( 'NONE',  ( -2.842019651049983331, 3.364325185445997679, 61.98378871700000303 ) ) ;
#5549 = CARTESIAN_POINT ( 'NONE',  ( -35.05918829505000645, 27.97290950744599769, 58.85000000000000142 ) ) ;
#5550 = DIRECTION ( 'NONE',  ( 0.000000000000000000, 1.000000000000000000, 0.000000000000000000 ) ) ;
#5551 = CARTESIAN_POINT ( 'NONE',  ( -30.48673169511680214, 10.97290950744599947, 7.250000000000000000 ) ) ;
#5552 = EDGE_LOOP ( 'NONE', ( #4530, #3955, #8101, #6972, #3715 ) ) ;
#5553 = VECTOR ( 'NONE', #8591, 1000.000000000000000 ) ;
#5554 = AXIS2_PLACEMENT_3D ( 'NONE', #11844, #12684, #2365 ) ;
#5555 = EDGE_CURVE ( 'NONE', #3595, #10924, #2565, .T. ) ;
#5556 = ORIENTED_EDGE ( 'NONE', *, *, #13260, .F. ) ;
#5557 = DIRECTION ( 'NONE',  ( -2.529805069132845816E-16, 1.000000000000000000, 0.000000000000000000 ) ) ;
#5558 = ADVANCED_FACE ( 'NONE', ( #1350 ), #2101, .T. ) ;
#5559 = VERTEX_POINT ( 'NONE', #11066 ) ;
#5560 = FACE_OUTER_BOUND ( 'NONE', #7527, .T. ) ;
#5561 = VERTEX_POINT ( 'NONE', #3799 ) ;
#5562 = CARTESIAN_POINT ( 'NONE',  ( 0.000000000000000000, 0.000000000000000000, 7.000000000000000000 ) ) ;
#5563 = PLANE ( 'NONE',  #12226 ) ;
#5564 = CARTESIAN_POINT ( 'NONE',  ( -16.08092853089235774, 4.500000000000000000, 11.23781208254507824 ) ) ;
#5565 = CIRCLE ( 'NONE', #2031, 7.618085573000000110 ) ;
#5566 = AXIS2_PLACEMENT_3D ( 'NONE', #5956, #9261, #8073 ) ;
#5567 = FACE_BOUND ( 'NONE', #12158, .T. ) ;
#5568 = DIRECTION ( 'NONE',  ( 0.000000000000000000, 0.000000000000000000, 1.000000000000000000 ) ) ;
#5569 = DIRECTION ( 'NONE',  ( -0.7071067811865500152, 8.659560562354959975E-17, 0.7071067811865450192 ) ) ;
#5570 = DIRECTION ( 'NONE',  ( 0.000000000000000000, 0.000000000000000000, 1.000000000000000000 ) ) ;
#5571 = CARTESIAN_POINT ( 'NONE',  ( 84.99521369064696330, 82.14063840035363739, 10.00000000000000000 ) ) ;
#5572 = AXIS2_PLACEMENT_3D ( 'NONE', #1824, #13679, #7108 ) ;
#5573 = AXIS2_PLACEMENT_3D ( 'NONE', #11701, #5396, #6384 ) ;
#5574 = VECTOR ( 'NONE', #5429, 1000.000000000000000 ) ;
#5575 = CARTESIAN_POINT ( 'NONE',  ( -17.01680957860132537, 30.33693478204560989, 53.15683758623448085 ) ) ;
#5576 = VERTEX_POINT ( 'NONE', #13289 ) ;
#5577 = ADVANCED_FACE ( 'NONE', ( #1843 ), #10356, .F. ) ;
#5578 = EDGE_CURVE ( 'NONE', #1000, #9989, #9247, .T. ) ;
#5579 = VERTEX_POINT ( 'NONE', #7973 ) ;
#5580 = FACE_OUTER_BOUND ( 'NONE', #12599, .T. ) ;
#5581 = CYLINDRICAL_SURFACE ( 'NONE', #11859, 0.7500000000000006661 ) ;
#5582 = ORIENTED_EDGE ( 'NONE', *, *, #9638, .T. ) ;
#5583 = LINE ( 'NONE', #3369, #4439 ) ;
#5584 = VECTOR ( 'NONE', #1017, 1000.000000000000000 ) ;
#5585 = CIRCLE ( 'NONE', #13398, 23.22993838181874793 ) ;
#5586 = CONICAL_SURFACE ( 'NONE', #4274, 4.250000000000000000, 0.7853981633974518317 ) ;
#5587 = CYLINDRICAL_SURFACE ( 'NONE', #8259, 0.7500000000000006661 ) ;
#5588 = CARTESIAN_POINT ( 'NONE',  ( -40.33164489498318517, 10.97290950744599947, 17.25000000000000000 ) ) ;
#5589 = ORIENTED_EDGE ( 'NONE', *, *, #7839, .F. ) ;
#5590 = AXIS2_PLACEMENT_3D ( 'NONE', #1744, #11454, #7040 ) ;
#5591 = ORIENTED_EDGE ( 'NONE', *, *, #11274, .F. ) ;
#5592 = DIRECTION ( 'NONE',  ( -0.000000000000000000, -0.000000000000000000, -1.000000000000000000 ) ) ;
#5593 = CIRCLE ( 'NONE', #693, 17.66282263685195275 ) ;
#5594 = AXIS2_PLACEMENT_3D ( 'NONE', #729, #2997, #2853 ) ;
#5595 = VERTEX_POINT ( 'NONE', #11206 ) ;
#5596 = EDGE_CURVE ( 'NONE', #586, #10750, #737, .T. ) ;
#5597 = EDGE_LOOP ( 'NONE', ( #7049, #4290, #9346, #2768 ) ) ;
#5598 = ORIENTED_EDGE ( 'NONE', *, *, #1847, .T. ) ;
#5599 = EDGE_CURVE ( 'NONE', #3420, #5468, #7195, .T. ) ;
#5600 = CARTESIAN_POINT ( 'NONE',  ( -0.04028432657539327000, 4.500000000000000000, 18.54539866546729243 ) ) ;
#5601 = CARTESIAN_POINT ( 'NONE',  ( -11.74835982676941981, -4.028726038184999858, 63.45000000000000284 ) ) ;
#5602 = ORIENTED_EDGE ( 'NONE', *, *, #4784, .F. ) ;
#5603 = EDGE_CURVE ( 'NONE', #3000, #12928, #11672, .T. ) ;
#5604 = CARTESIAN_POINT ( 'NONE',  ( -18.05918829504999934, 10.97290950744599947, 61.25000000000000000 ) ) ;
#5605 = DIRECTION ( 'NONE',  ( 0.000000000000000000, 0.000000000000000000, 1.000000000000000000 ) ) ;
#5606 = FACE_BOUND ( 'NONE', #2967, .T. ) ;
#5607 = EDGE_CURVE ( 'NONE', #3428, #6986, #305, .T. ) ;
#5608 = CARTESIAN_POINT ( 'NONE',  ( -3.759188295049999518, 27.97290950744599769, 58.85000000000000142 ) ) ;
#5609 = AXIS2_PLACEMENT_3D ( 'NONE', #4193, #8439, #7305 ) ;
#5610 = EDGE_CURVE ( 'NONE', #9493, #7236, #12569, .T. ) ;
#5611 = CIRCLE ( 'NONE', #6287, 5.000000000000000888 ) ;
#5612 = AXIS2_PLACEMENT_3D ( 'NONE', #9154, #13477, #1609 ) ;
#5613 = ORIENTED_EDGE ( 'NONE', *, *, #13379, .F. ) ;
#5614 = ADVANCED_FACE ( 'NONE', ( #1560 ), #518, .F. ) ;
#5615 = AXIS2_PLACEMENT_3D ( 'NONE', #4113, #4243, #2026 ) ;
#5616 = CARTESIAN_POINT ( 'NONE',  ( 86.99521369064697751, 82.14063840035363739, 10.00000000000000000 ) ) ;
#5617 = ORIENTED_EDGE ( 'NONE', *, *, #2556, .F. ) ;
#5618 = LINE ( 'NONE', #4515, #12994 ) ;
#5619 = ADVANCED_FACE ( 'NONE', ( #5810 ), #4545, .T. ) ;
#5620 = CARTESIAN_POINT ( 'NONE',  ( -21.29502067386963304, 30.13379967401889203, 55.02888677376879656 ) ) ;
#5621 = SURFACE_STYLE_USAGE ( .BOTH. , #6671 ) ;
#5622 = ORIENTED_EDGE ( 'NONE', *, *, #5607, .T. ) ;
#5623 = CARTESIAN_POINT ( 'NONE',  ( 142.6356359024541973, 87.03908161011133870, 20.00000000000000000 ) ) ;
#5624 = CARTESIAN_POINT ( 'NONE',  ( 68.49370948373500312, 85.78908161011133870, 0.000000000000000000 ) ) ;
#5625 = CARTESIAN_POINT ( 'NONE',  ( -19.71317847370539766, 12.84756053868127879, 53.85000000000000142 ) ) ;
#5626 = ADVANCED_FACE ( 'NONE', ( #12388 ), #11271, .T. ) ;
#5627 = CARTESIAN_POINT ( 'NONE',  ( -25.73489962141544751, -4.139534227248430120, 61.65000000000000568 ) ) ;
#5628 = ORIENTED_EDGE ( 'NONE', *, *, #2385, .F. ) ;
#5629 = CIRCLE ( 'NONE', #965, 8.300000000000000711 ) ;
#5630 = EDGE_LOOP ( 'NONE', ( #974, #1082 ) ) ;
#5631 = LINE ( 'NONE', #9912, #7452 ) ;
#5632 = CARTESIAN_POINT ( 'NONE',  ( 76.18094369249178044, 97.20665973629650125, 10.00000000000000000 ) ) ;
#5633 = FACE_OUTER_BOUND ( 'NONE', #163, .T. ) ;
#5634 =( NAMED_UNIT ( * ) SI_UNIT ( $, .STERADIAN. ) SOLID_ANGLE_UNIT ( ) );
#5635 = FACE_OUTER_BOUND ( 'NONE', #9619, .T. ) ;
#5636 = FACE_OUTER_BOUND ( 'NONE', #12012, .T. ) ;
#5637 = LINE ( 'NONE', #11034, #6951 ) ;
#5638 = FACE_OUTER_BOUND ( 'NONE', #10837, .T. ) ;
#5639 = LINE ( 'NONE', #4542, #9843 ) ;
#5640 = EDGE_CURVE ( 'NONE', #2414, #8708, #2096, .T. ) ;
#5641 = CARTESIAN_POINT ( 'NONE',  ( 141.8856359024541973, 110.7284214383315089, 0.000000000000000000 ) ) ;
#5642 = PLANE ( 'NONE',  #9345 ) ;
#5643 = AXIS2_PLACEMENT_3D ( 'NONE', #6897, #2599, #13320 ) ;
#5644 = EDGE_LOOP ( 'NONE', ( #420, #10734, #6410, #6330 ) ) ;
#5645 = ORIENTED_EDGE ( 'NONE', *, *, #4185, .F. ) ;
#5646 = FACE_OUTER_BOUND ( 'NONE', #5552, .T. ) ;
#5647 = VERTEX_POINT ( 'NONE', #10098 ) ;
#5648 = DIRECTION ( 'NONE',  ( 1.000000000000000000, 0.000000000000000000, 0.000000000000000000 ) ) ;
#5649 = LINE ( 'NONE', #12915, #2708 ) ;
#5650 = DIRECTION ( 'NONE',  ( 0.000000000000000000, 0.000000000000000000, -1.000000000000000000 ) ) ;
#5651 = LINE ( 'NONE', #6976, #9122 ) ;
#5652 = DIRECTION ( 'NONE',  ( 0.000000000000000000, 0.000000000000000000, -1.000000000000000000 ) ) ;
#5653 = DIRECTION ( 'NONE',  ( -0.6615960714621564875, 0.7498604124941129490, 0.000000000000000000 ) ) ;
#5654 = ADVANCED_FACE ( 'NONE', ( #4780 ), #2909, .T. ) ;
#5655 = EDGE_CURVE ( 'NONE', #9588, #8303, #2331, .T. ) ;
#5656 = ORIENTED_EDGE ( 'NONE', *, *, #1753, .T. ) ;
#5657 = EDGE_CURVE ( 'NONE', #6644, #1261, #969, .T. ) ;
#5658 = ORIENTED_EDGE ( 'NONE', *, *, #12696, .T. ) ;
#5659 = DIRECTION ( 'NONE',  ( 0.000000000000000000, 1.000000000000000000, 0.000000000000000000 ) ) ;
#5660 = ORIENTED_EDGE ( 'NONE', *, *, #8157, .F. ) ;
#5661 = ORIENTED_EDGE ( 'NONE', *, *, #13260, .T. ) ;
#5662 = ORIENTED_EDGE ( 'NONE', *, *, #9557, .F. ) ;
#5663 = VERTEX_POINT ( 'NONE', #9093 ) ;
#5664 = LINE ( 'NONE', #3521, #9778 ) ;
#5665 = ORIENTED_EDGE ( 'NONE', *, *, #10254, .F. ) ;
#5666 = DIRECTION ( 'NONE',  ( -0.6615960714621564875, 0.7498604124941129490, 0.000000000000000000 ) ) ;
#5667 = CARTESIAN_POINT ( 'NONE',  ( -17.37706816261102105, 26.95825899741793563, 56.01342904187733041 ) ) ;
#5668 = CARTESIAN_POINT ( 'NONE',  ( 116.7775623211734342, 112.2890816101113387, 20.00000000000000000 ) ) ;
#5669 = DIRECTION ( 'NONE',  ( 0.000000000000000000, 0.000000000000000000, -1.000000000000000000 ) ) ;
#5670 = EDGE_CURVE ( 'NONE', #1784, #3590, #1178, .T. ) ;
#5671 = AXIS2_PLACEMENT_3D ( 'NONE', #12103, #4827, #5869 ) ;
#5672 =( BOUNDED_CURVE ( )  B_SPLINE_CURVE ( 3, ( #1894, #829, #1966, #3920 ),
 .UNSPECIFIED., .F., .F. ) 
 B_SPLINE_CURVE_WITH_KNOTS ( ( 4, 4 ),
 ( 1.570796326794896558, 3.141592653589793116 ),
 .UNSPECIFIED. ) 
 CURVE ( )  GEOMETRIC_REPRESENTATION_ITEM ( )  RATIONAL_B_SPLINE_CURVE ( ( 1.000000000000000000, 0.8047378541243649375, 0.8047378541243649375, 1.000000000000000000 ) ) 
 REPRESENTATION_ITEM ( '' )  );
#5673 = ORIENTED_EDGE ( 'NONE', *, *, #1286, .T. ) ;
#5674 = DIRECTION ( 'NONE',  ( -1.000000000000000000, 0.000000000000000000, 0.000000000000000000 ) ) ;
#5675 = VERTEX_POINT ( 'NONE', #6997 ) ;
#5676 = VECTOR ( 'NONE', #114, 1000.000000000000000 ) ;
#5677 = CARTESIAN_POINT ( 'NONE',  ( -21.69765923394618667, 30.07360145807689733, 58.70649103051356121 ) ) ;
#5678 =( NAMED_UNIT ( * ) PLANE_ANGLE_UNIT ( ) SI_UNIT ( $, .RADIAN. ) );
#5679 = EDGE_LOOP ( 'NONE', ( #5739, #10634, #7247, #3155 ) ) ;
#5680 = LINE ( 'NONE', #9959, #3538 ) ;
#5681 = DIRECTION ( 'NONE',  ( -0.000000000000000000, -0.000000000000000000, -1.000000000000000000 ) ) ;
#5682 = FACE_BOUND ( 'NONE', #1529, .T. ) ;
#5683 = DIRECTION ( 'NONE',  ( -1.000000000000000000, 0.000000000000000000, 0.000000000000000000 ) ) ;
#5684 = PRODUCT_DEFINITION_SHAPE ( 'NONE', 'NONE',  #7890 ) ;
#5685 = DIRECTION ( 'NONE',  ( 1.000000000000000000, 0.000000000000000000, 0.000000000000000000 ) ) ;
#5686 = EDGE_CURVE ( 'NONE', #6919, #9237, #8725, .T. ) ;
#5687 = ADVANCED_FACE ( 'NONE', ( #1174 ), #4469, .F. ) ;
#5688 = VECTOR ( 'NONE', #12827, 1000.000000000000000 ) ;
#5689 = VERTEX_POINT ( 'NONE', #2251 ) ;
#5690 = EDGE_CURVE ( 'NONE', #10270, #12491, #5415, .T. ) ;
#5691 = ORIENTED_EDGE ( 'NONE', *, *, #3225, .F. ) ;
#5692 = FACE_OUTER_BOUND ( 'NONE', #9770, .T. ) ;
#5693 = DIRECTION ( 'NONE',  ( 0.000000000000000000, 0.000000000000000000, -1.000000000000000000 ) ) ;
#5694 = EDGE_LOOP ( 'NONE', ( #8368, #7530 ) ) ;
#5695 = DIRECTION ( 'NONE',  ( -0.000000000000000000, -0.000000000000000000, 1.000000000000000000 ) ) ;
#5696 = SURFACE_STYLE_FILL_AREA ( #13312 ) ;
#5697 = CARTESIAN_POINT ( 'NONE',  ( -5.309188295050000228, 27.97290950744599769, 58.85000000000000142 ) ) ;
#5698 = FACE_OUTER_BOUND ( 'NONE', #13598, .T. ) ;
#5699 = CARTESIAN_POINT ( 'NONE',  ( -18.05918829504999934, 10.97290950744599947, 53.85000000000000142 ) ) ;
#5700 = CARTESIAN_POINT ( 'NONE',  ( 5.999999999999999112, -12.00000000000000178, 7.000000000000000000 ) ) ;
#5701 = DIRECTION ( 'NONE',  ( -0.000000000000000000, -0.000000000000000000, 1.000000000000000000 ) ) ;
#5702 = CARTESIAN_POINT ( 'NONE',  ( -10.78334210919089919, 29.19143287883919768, 64.85000000000000853 ) ) ;
#5703 = CIRCLE ( 'NONE', #7925, 16.72262947720610171 ) ;
#5704 = FACE_BOUND ( 'NONE', #5630, .T. ) ;
#5705 = LINE ( 'NONE', #9006, #8224 ) ;
#5706 = EDGE_CURVE ( 'NONE', #506, #87, #8538, .T. ) ;
#5707 = EDGE_CURVE ( 'NONE', #8370, #11045, #12594, .T. ) ;
#5708 = EDGE_LOOP ( 'NONE', ( #5731, #10396, #9824, #13278 ) ) ;
#5709 = VECTOR ( 'NONE', #2054, 1000.000000000000114 ) ;
#5710 = ADVANCED_FACE ( 'NONE', ( #9706 ), #6556, .F. ) ;
#5711 = ORIENTED_EDGE ( 'NONE', *, *, #12535, .T. ) ;
#5712 = CARTESIAN_POINT ( 'NONE',  ( 44.63563590245421864, 85.03908161011133870, 0.7500000000000006661 ) ) ;
#5713 = ORIENTED_EDGE ( 'NONE', *, *, #8545, .T. ) ;
#5714 = ORIENTED_EDGE ( 'NONE', *, *, #511, .T. ) ;
#5715 = CYLINDRICAL_SURFACE ( 'NONE', #8183, 3.000000000000000000 ) ;
#5716 = DIRECTION ( 'NONE',  ( -0.000000000000000000, -0.000000000000000000, 1.000000000000000000 ) ) ;
#5717 = FACE_OUTER_BOUND ( 'NONE', #1832, .T. ) ;
#5718 = CARTESIAN_POINT ( 'NONE',  ( -18.05918829504999934, 10.97290950744599947, 61.65955166399999854 ) ) ;
#5719 = AXIS2_PLACEMENT_3D ( 'NONE', #4692, #9070, #5648 ) ;
#5720 = CARTESIAN_POINT ( 'NONE',  ( -18.05918829504999934, 10.97290950744599947, 30.59999999999999787 ) ) ;
#5721 = VERTEX_POINT ( 'NONE', #1909 ) ;
#5722 = ORIENTED_EDGE ( 'NONE', *, *, #3146, .T. ) ;
#5723 = EDGE_LOOP ( 'NONE', ( #6363, #13273, #10378, #8766 ) ) ;
#5724 = DIRECTION ( 'NONE',  ( 0.000000000000000000, 0.000000000000000000, 1.000000000000000000 ) ) ;
#5725 = EDGE_LOOP ( 'NONE', ( #509, #10764, #3789, #3102, #3409 ) ) ;
#5726 = ORIENTED_EDGE ( 'NONE', *, *, #3672, .F. ) ;
#5727 = AXIS2_PLACEMENT_3D ( 'NONE', #8719, #3423, #9639 ) ;
#5728 = DIRECTION ( 'NONE',  ( 1.000000000000000000, 0.000000000000000000, 0.000000000000000000 ) ) ;
#5729 = EDGE_CURVE ( 'NONE', #5077, #10024, #2780, .T. ) ;
#5730 = CARTESIAN_POINT ( 'NONE',  ( -11.91335496205000055, 10.97290950744599947, 60.60999999999999943 ) ) ;
#5731 = ORIENTED_EDGE ( 'NONE', *, *, #8691, .F. ) ;
#5732 = CARTESIAN_POINT ( 'NONE',  ( -11.75918829505000041, 10.97290950744599947, 63.02000000000000313 ) ) ;
#5733 = CARTESIAN_POINT ( 'NONE',  ( -12.00918829505000041, 10.97290950744599947, 64.85000000000000853 ) ) ;
#5734 = DIRECTION ( 'NONE',  ( 0.000000000000000000, 0.000000000000000000, -1.000000000000000000 ) ) ;
#5735 = DIRECTION ( 'NONE',  ( 0.4528443260392610026, 0.8915896008669278450, 0.000000000000000000 ) ) ;
#5736 = CIRCLE ( 'NONE', #12224, 1.999999999999989564 ) ;
#5737 = CIRCLE ( 'NONE', #13549, 4.750000000000000888 ) ;
#5738 = PRESENTATION_LAYER_ASSIGNMENT (  '', '', ( #11770 ) ) ;
#5739 = ORIENTED_EDGE ( 'NONE', *, *, #10464, .F. ) ;
#5740 = ADVANCED_BREP_SHAPE_REPRESENTATION ( '', ( #4487, #6434 ), #10026 ) ;
#5741 = ADVANCED_FACE ( 'NONE', ( #10496 ), #8998, .F. ) ;
#5742 = DIRECTION ( 'NONE',  ( 0.000000000000000000, 0.000000000000000000, 1.000000000000000000 ) ) ;
#5743 = ORIENTED_EDGE ( 'NONE', *, *, #2016, .T. ) ;
#5744 = CIRCLE ( 'NONE', #9097, 16.95000000000000284 ) ;
#5745 = AXIS2_PLACEMENT_3D ( 'NONE', #9669, #9808, #3253 ) ;
#5746 = CIRCLE ( 'NONE', #13564, 1.999999999999996669 ) ;
#5747 = EDGE_CURVE ( 'NONE', #11638, #1281, #11233, .T. ) ;
#5748 = CARTESIAN_POINT ( 'NONE',  ( 0.000000000000000000, 0.000000000000000000, 23.00000000000000000 ) ) ;
#5749 = AXIS2_PLACEMENT_3D ( 'NONE', #10785, #1200, #12742 ) ;
#5750 = CARTESIAN_POINT ( 'NONE',  ( -20.72664669423063089, 30.20666037455253061, 60.46838943485088436 ) ) ;
#5751 = DIRECTION ( 'NONE',  ( 0.000000000000000000, 0.000000000000000000, 1.000000000000000000 ) ) ;
#5752 = DIRECTION ( 'NONE',  ( -1.000000000000000000, 0.000000000000000000, 0.000000000000000000 ) ) ;
#5753 = CARTESIAN_POINT ( 'NONE',  ( -23.41085226126194740, -11.41022146549009975, 64.85000000000000853 ) ) ;
#5754 = DIRECTION ( 'NONE',  ( 0.000000000000000000, 0.000000000000000000, 1.000000000000000000 ) ) ;
#5755 = LINE ( 'NONE', #9837, #6234 ) ;
#5756 =( LENGTH_UNIT ( ) NAMED_UNIT ( * ) SI_UNIT ( .MILLI., .METRE. ) );
#5757 = ORIENTED_EDGE ( 'NONE', *, *, #13395, .T. ) ;
#5758 = CIRCLE ( 'NONE', #2000, 0.5000000000000004441 ) ;
#5759 = CIRCLE ( 'NONE', #9570, 6.450000000000009948 ) ;
#5760 = CIRCLE ( 'NONE', #3325, 1.999999999999989564 ) ;
#5761 = AXIS2_PLACEMENT_3D ( 'NONE', #6929, #781, #11268 ) ;
#5762 = ORIENTED_EDGE ( 'NONE', *, *, #11947, .F. ) ;
#5763 = DIRECTION ( 'NONE',  ( 1.000000000000000000, 0.000000000000000000, 0.000000000000000000 ) ) ;
#5764 = CARTESIAN_POINT ( 'NONE',  ( -35.05918829505000645, -6.027090492554000534, 58.85000000000000142 ) ) ;
#5765 = FACE_OUTER_BOUND ( 'NONE', #9954, .T. ) ;
#5766 = EDGE_CURVE ( 'NONE', #4982, #12198, #9774, .T. ) ;
#5767 = LINE ( 'NONE', #12143, #13099 ) ;
#5768 = PLANE ( 'NONE',  #1745 ) ;
#5769 = FACE_OUTER_BOUND ( 'NONE', #5391, .T. ) ;
#5770 = AXIS2_PLACEMENT_3D ( 'NONE', #6879, #390, #12271 ) ;
#5771 = CARTESIAN_POINT ( 'NONE',  ( -40.05918829505000645, 35.97290950744599769, 10.00000000000000000 ) ) ;
#5772 = CARTESIAN_POINT ( 'NONE',  ( -1.059188295049996231, -6.027090492554000534, 5.250000000000000000 ) ) ;
#5773 = CARTESIAN_POINT ( 'NONE',  ( -5.631644894983189431, 10.97290950744599947, 17.25000000000000000 ) ) ;
#5774 = DIRECTION ( 'NONE',  ( 1.000000000000000000, 0.000000000000000000, 0.000000000000000000 ) ) ;
#5775 = ADVANCED_FACE ( 'NONE', ( #11876 ), #6082, .T. ) ;
#5776 = CARTESIAN_POINT ( 'NONE',  ( -1.059188295049996231, 27.97290950744599769, 0.000000000000000000 ) ) ;
#5777 = AXIS2_PLACEMENT_3D ( 'NONE', #2913, #3804, #9035 ) ;
#5778 = PLANE ( 'NONE',  #10017 ) ;
#5779 = ADVANCED_FACE ( 'NONE', ( #4397 ), #8331, .F. ) ;
#5780 = ORIENTED_EDGE ( 'NONE', *, *, #9645, .T. ) ;
#5781 = AXIS2_PLACEMENT_3D ( 'NONE', #6734, #2566, #11067 ) ;
#5782 = VERTEX_POINT ( 'NONE', #7587 ) ;
#5783 = DIRECTION ( 'NONE',  ( 0.000000000000000000, 0.000000000000000000, -1.000000000000000000 ) ) ;
#5784 = ORIENTED_EDGE ( 'NONE', *, *, #4447, .F. ) ;
#5786 = ORIENTED_EDGE ( 'NONE', *, *, #11186, .F. ) ;
#5785 = EDGE_CURVE ( 'NONE', #918, #2345, #13560, .T. ) ;
#5787 = DIRECTION ( 'NONE',  ( -0.000000000000000000, -0.000000000000000000, 1.000000000000000000 ) ) ;
#5788 = CYLINDRICAL_SURFACE ( 'NONE', #5612, 2.000000000000001776 ) ;
#5789 = CARTESIAN_POINT ( 'NONE',  ( -18.05918829504999934, 10.00028003023991907, 62.14999999999999858 ) ) ;
#5790 = CARTESIAN_POINT ( 'NONE',  ( -41.50918829505000218, 27.97290950744599769, 17.25000000000000000 ) ) ;
#5791 = CARTESIAN_POINT ( 'NONE',  ( 86.99521369064697751, 82.14063840035363739, 20.00000000000000000 ) ) ;
#5792 = CARTESIAN_POINT ( 'NONE',  ( -1.059188295049996231, -6.027090492554000534, 17.25000000000000000 ) ) ;
#5793 = EDGE_CURVE ( 'NONE', #11959, #9990, #9667, .T. ) ;
#5794 = DIRECTION ( 'NONE',  ( 0.000000000000000000, 0.000000000000000000, -1.000000000000000000 ) ) ;
#5795 = VECTOR ( 'NONE', #13481, 1000.000000000000000 ) ;
#5796 = VERTEX_POINT ( 'NONE', #8260 ) ;
#5797 = DIRECTION ( 'NONE',  ( 0.000000000000000000, 0.000000000000000000, 1.000000000000000000 ) ) ;
#5798 = VERTEX_POINT ( 'NONE', #8574 ) ;
#5799 = AXIS2_PLACEMENT_3D ( 'NONE', #13586, #4037, #8292 ) ;
#5800 = EDGE_LOOP ( 'NONE', ( #3385, #8533, #8962, #10638 ) ) ;
#5801 = AXIS2_PLACEMENT_3D ( 'NONE', #2735, #12208, #3564 ) ;
#5802 = VECTOR ( 'NONE', #13562, 1000.000000000000000 ) ;
#5803 = FACE_OUTER_BOUND ( 'NONE', #11478, .T. ) ;
#5804 = CIRCLE ( 'NONE', #10968, 16.00000000000000000 ) ;
#5805 = ORIENTED_EDGE ( 'NONE', *, *, #2482, .F. ) ;
#5806 = CARTESIAN_POINT ( 'NONE',  ( -33.27635693905001801, 18.58149382944601058, 61.98378871700000303 ) ) ;
#5807 = LINE ( 'NONE', #13078, #10233 ) ;
#5808 = EDGE_LOOP ( 'NONE', ( #8436, #4772 ) ) ;
#5809 = CARTESIAN_POINT ( 'NONE',  ( -18.05918829430469685, 19.27290950744890097, 63.15000000009349179 ) ) ;
#5810 = FACE_OUTER_BOUND ( 'NONE', #12392, .T. ) ;
#5811 = CARTESIAN_POINT ( 'NONE',  ( -38.05918829505000645, -6.027090492554000534, 10.00000000000000000 ) ) ;
#5812 = EDGE_CURVE ( 'NONE', #54, #5796, #11472, .T. ) ;
#5813 = FACE_BOUND ( 'NONE', #6012, .T. ) ;
#5814 = VECTOR ( 'NONE', #403, 1000.000000000000000 ) ;
#5815 = AXIS2_PLACEMENT_3D ( 'NONE', #5974, #13255, #3695 ) ;
#5816 = ORIENTED_EDGE ( 'NONE', *, *, #2180, .T. ) ;
#5817 = VERTEX_POINT ( 'NONE', #849 ) ;
#5818 = CARTESIAN_POINT ( 'NONE',  ( -18.05918829504999934, 10.97290950744599947, 57.35000000000000142 ) ) ;
#5819 = VERTEX_POINT ( 'NONE', #9383 ) ;
#5820 = DIRECTION ( 'NONE',  ( 0.000000000000000000, 0.000000000000000000, -1.000000000000000000 ) ) ;
#5821 = CARTESIAN_POINT ( 'NONE',  ( -21.24216064964741690, 30.14123926836247591, 59.76621780875206014 ) ) ;
#5822 = VECTOR ( 'NONE', #13609, 1000.000000000000000 ) ;
#5823 = AXIS2_PLACEMENT_3D ( 'NONE', #3408, #13788, #7701 ) ;
#5824 = CARTESIAN_POINT ( 'NONE',  ( -3.999999999999998224, -1.301042606982605321E-15, 0.000000000000000000 ) ) ;
#5825 = CARTESIAN_POINT ( 'NONE',  ( 50.38563590245420443, 104.1554980190242361, 23.00000000000000000 ) ) ;
#5826 = AXIS2_PLACEMENT_3D ( 'NONE', #5954, #460, #1708 ) ;
#5827 = LINE ( 'NONE', #10112, #5504 ) ;
#5828 = FACE_OUTER_BOUND ( 'NONE', #10292, .T. ) ;
#5829 = CYLINDRICAL_SURFACE ( 'NONE', #2918, 3.000000000000002665 ) ;
#5830 =( NAMED_UNIT ( * ) SI_UNIT ( $, .STERADIAN. ) SOLID_ANGLE_UNIT ( ) );
#5831 = EDGE_CURVE ( 'NONE', #13422, #11802, #5183, .T. ) ;
#5832 = EDGE_CURVE ( 'NONE', #11639, #9038, #13019, .T. ) ;
#5833 = STYLED_ITEM ( 'NONE', ( #7435 ), #4601 ) ;
#5834 = EDGE_CURVE ( 'NONE', #10854, #7101, #1189, .T. ) ;
#5835 = EDGE_LOOP ( 'NONE', ( #10374, #5247, #13510, #10923 ) ) ;
#5836 = DIRECTION ( 'NONE',  ( 0.000000000000000000, 0.000000000000000000, 1.000000000000000000 ) ) ;
#5837 = FACE_OUTER_BOUND ( 'NONE', #12513, .T. ) ;
#5838 = VERTEX_POINT ( 'NONE', #9922 ) ;
#5839 = CARTESIAN_POINT ( 'NONE',  ( -35.05918829505000645, 27.97290950744599769, 5.250000000000000000 ) ) ;
#5840 = CARTESIAN_POINT ( 'NONE',  ( -18.05918829504999934, 10.97290950744599947, 60.85000000000000142 ) ) ;
#5841 = CARTESIAN_POINT ( 'NONE',  ( -18.05918829504999934, 10.97290950744599947, 53.85000000000000142 ) ) ;
#5842 = CARTESIAN_POINT ( 'NONE',  ( 109.1537879975201406, 82.61803701715820125, 20.00000000000000000 ) ) ;
#5843 = FACE_OUTER_BOUND ( 'NONE', #11818, .T. ) ;
#5844 = DIRECTION ( 'NONE',  ( 0.000000000000000000, 0.000000000000000000, -1.000000000000000000 ) ) ;
#5845 = DIRECTION ( 'NONE',  ( -0.000000000000000000, 0.000000000000000000, 1.000000000000000000 ) ) ;
#5846 = CIRCLE ( 'NONE', #2077, 24.92993838181874722 ) ;
#5847 = CARTESIAN_POINT ( 'NONE',  ( 142.6356359024541973, 111.0390816101113245, 0.7500000000000006661 ) ) ;
#5848 = CARTESIAN_POINT ( 'NONE',  ( 4.000000000000001776, -4.336808689942017736E-16, 0.000000000000000000 ) ) ;
#5849 = ADVANCED_FACE ( 'NONE', ( #8793 ), #11101, .T. ) ;
#5850 = EDGE_LOOP ( 'NONE', ( #2707, #11125 ) ) ;
#5851 = EDGE_LOOP ( 'NONE', ( #3737, #10185, #13643, #2747 ) ) ;
#5852 = EDGE_CURVE ( 'NONE', #1, #13705, #11682, .T. ) ;
#5853 = AXIS2_PLACEMENT_3D ( 'NONE', #4635, #5527, #11904 ) ;
#5854 = CARTESIAN_POINT ( 'NONE',  ( -20.70557258089865016, 13.97235115742243927, 30.59999999999999787 ) ) ;
#5855 = ORIENTED_EDGE ( 'NONE', *, *, #10569, .F. ) ;
#5856 = VERTEX_POINT ( 'NONE', #12291 ) ;
#5857 = CARTESIAN_POINT ( 'NONE',  ( -16.60019635188397658, 27.03346355975618565, 56.97665238683693190 ) ) ;
#5858 = CARTESIAN_POINT ( 'NONE',  ( 0.04028432657539327000, 4.500000000000000000, -18.54539866546729243 ) ) ;
#5859 = DIRECTION ( 'NONE',  ( 0.000000000000000000, 0.000000000000000000, -1.000000000000000000 ) ) ;
#5860 = DIRECTION ( 'NONE',  ( -0.000000000000000000, -0.000000000000000000, 1.000000000000000000 ) ) ;
#5861 = CARTESIAN_POINT ( 'NONE',  ( -18.05918829504999934, 10.97290950744599947, 60.60999999999999943 ) ) ;
#5862 = FACE_OUTER_BOUND ( 'NONE', #9661, .T. ) ;
#5863 = CARTESIAN_POINT ( 'NONE',  ( -1.059188295049996231, 27.97290950744599769, 7.250000000000000000 ) ) ;
#5864 = AXIS2_PLACEMENT_3D ( 'NONE', #11133, #13227, #4914 ) ;
#5865 = EDGE_CURVE ( 'NONE', #7102, #1633, #12579, .T. ) ;
#5866 = ORIENTED_EDGE ( 'NONE', *, *, #2244, .F. ) ;
#5867 = EDGE_CURVE ( 'NONE', #533, #2781, #8550, .T. ) ;
#5868 = ORIENTED_EDGE ( 'NONE', *, *, #6387, .F. ) ;
#5869 = DIRECTION ( 'NONE',  ( 0.000000000000000000, 0.000000000000000000, 1.000000000000000000 ) ) ;
#5870 = ORIENTED_EDGE ( 'NONE', *, *, #12293, .F. ) ;
#5871 = ORIENTED_EDGE ( 'NONE', *, *, #5181, .F. ) ;
#5872 = ADVANCED_FACE ( 'NONE', ( #10062 ), #3765, .F. ) ;
#5873 = AXIS2_PLACEMENT_3D ( 'NONE', #8091, #6056, #5151 ) ;
#5874 = DIRECTION ( 'NONE',  ( 1.000000000000000000, 0.000000000000000000, 0.000000000000000000 ) ) ;
#5875 = ORIENTED_EDGE ( 'NONE', *, *, #2829, .T. ) ;
#5876 = CARTESIAN_POINT ( 'NONE',  ( -15.54654308236029792, 19.85770471824265115, 64.85000000000000853 ) ) ;
#5877 = DIRECTION ( 'NONE',  ( 0.000000000000000000, 1.000000000000000000, 0.000000000000000000 ) ) ;
#5878 = FACE_OUTER_BOUND ( 'NONE', #12236, .T. ) ;
#5879 = CYLINDRICAL_SURFACE ( 'NONE', #9414, 1.725000000000000755 ) ;
#5880 = CARTESIAN_POINT ( 'NONE',  ( -18.05918829504999934, 10.97290950744599947, 116.8499999999999943 ) ) ;
#5881 = CARTESIAN_POINT ( 'NONE',  ( 140.6356359024541973, 108.9054980190242503, 22.75000000000000000 ) ) ;
#5882 = CARTESIAN_POINT ( 'NONE',  ( 140.5320825118609207, 104.0090514096174843, 23.00000000000000000 ) ) ;
#5883 = EDGE_CURVE ( 'NONE', #8303, #936, #11460, .T. ) ;
#5884 = ORIENTED_EDGE ( 'NONE', *, *, #7641, .T. ) ;
#5885 = ORIENTED_EDGE ( 'NONE', *, *, #3455, .T. ) ;
#5886 = ORIENTED_EDGE ( 'NONE', *, *, #2760, .T. ) ;
#5887 = EDGE_CURVE ( 'NONE', #2257, #13584, #2466, .T. ) ;
#5888 = LINE ( 'NONE', #12585, #1246 ) ;
#5889 = DIRECTION ( 'NONE',  ( 0.000000000000000000, 0.000000000000000000, 1.000000000000000000 ) ) ;
#5890 = CARTESIAN_POINT ( 'NONE',  ( -21.06699515661435029, 30.16479851496719533, 60.03871598454315262 ) ) ;
#5891 = DIRECTION ( 'NONE',  ( 0.000000000000000000, 0.000000000000000000, 1.000000000000000000 ) ) ;
#5892 = CARTESIAN_POINT ( 'NONE',  ( 68.49370948373500312, 85.78908161011133870, 20.00000000000000000 ) ) ;
#5893 = CARTESIAN_POINT ( 'NONE',  ( -27.49999999999998934, 9.000000000000000000, -30.00000000000000355 ) ) ;
#5894 = DIRECTION ( 'NONE',  ( -1.000000000000000000, 0.000000000000000000, 0.000000000000000000 ) ) ;
#5895 = ORIENTED_EDGE ( 'NONE', *, *, #2502, .T. ) ;
#5896 = AXIS2_PLACEMENT_3D ( 'NONE', #2115, #3289, #1041 ) ;
#5897 = CARTESIAN_POINT ( 'NONE',  ( 116.7775623211734342, 112.2890816101113387, 20.00000000000000000 ) ) ;
#5898 =( REPRESENTATION_RELATIONSHIP ('NONE','NONE', #11848, #5062 ) REPRESENTATION_RELATIONSHIP_WITH_TRANSFORMATION ( #3261 )SHAPE_REPRESENTATION_RELATIONSHIP( ) );
#5899 = FACE_OUTER_BOUND ( 'NONE', #8075, .T. ) ;
#5900 = LINE ( 'NONE', #6956, #6248 ) ;
#5901 = DIRECTION ( 'NONE',  ( 0.000000000000000000, 0.000000000000000000, 1.000000000000000000 ) ) ;
#5902 = LINE ( 'NONE', #8402, #8646 ) ;
#5903 = CARTESIAN_POINT ( 'NONE',  ( -40.05918829504999934, -11.02709049255400053, 0.000000000000000000 ) ) ;
#5904 = CLOSED_SHELL ( 'NONE', ( #1965, #11164, #2409, #13657, #4308, #13050, #7932, #11655, #8241, #5229, #11071, #13376, #11086, #2114, #3263, #9132, #934, #6518, #8578, #891, #13014, #3259 ) ) ;
#5905 = CARTESIAN_POINT ( 'NONE',  ( 1.640811704950005057, -6.027090492554000534, 7.250000000000000000 ) ) ;
#5906 = DIRECTION ( 'NONE',  ( -1.000000000000000000, 0.000000000000000000, 0.000000000000000000 ) ) ;
#5907 = DIRECTION ( 'NONE',  ( 1.000000000000000000, 0.000000000000000000, 0.000000000000000000 ) ) ;
#5908 = EDGE_CURVE ( 'NONE', #13076, #4982, #2410, .T. ) ;
#5909 = DIRECTION ( 'NONE',  ( -0.000000000000000000, 1.000000000000000000, -0.000000000000000000 ) ) ;
#5910 = CARTESIAN_POINT ( 'NONE',  ( 140.6356359024541973, 108.9054980190242503, 22.89644660940672694 ) ) ;
#5911 = CARTESIAN_POINT ( 'NONE',  ( 5.999999999999999112, -12.00000000000000178, 0.000000000000000000 ) ) ;
#5912 = AXIS2_PLACEMENT_3D ( 'NONE', #11730, #5368, #9647 ) ;
#5913 = EDGE_LOOP ( 'NONE', ( #11744, #1481, #10995, #5966 ) ) ;
#5914 = DIRECTION ( 'NONE',  ( 0.000000000000000000, 0.000000000000000000, -1.000000000000000000 ) ) ;
#5915 = ORIENTED_EDGE ( 'NONE', *, *, #3856, .T. ) ;
#5916 = ORIENTED_EDGE ( 'NONE', *, *, #6474, .T. ) ;
#5917 = DIRECTION ( 'NONE',  ( 0.7071067811865451302, -0.7071067811865500152, -0.000000000000000000 ) ) ;
#5918 = AXIS2_PLACEMENT_3D ( 'NONE', #12062, #2522, #6755 ) ;
#5919 = DIRECTION ( 'NONE',  ( 1.000000000000000000, -0.000000000000000000, -0.000000000000000000 ) ) ;
#5920 = FACE_OUTER_BOUND ( 'NONE', #3264, .T. ) ;
#5921 = EDGE_CURVE ( 'NONE', #11822, #8835, #5228, .T. ) ;
#5922 = CARTESIAN_POINT ( 'NONE',  ( -18.05918829504999934, 19.27191034044600215, 63.13003331699999876 ) ) ;
#5923 = DIRECTION ( 'NONE',  ( 0.000000000000000000, 0.000000000000000000, -1.000000000000000000 ) ) ;
#5924 = CARTESIAN_POINT ( 'NONE',  ( 116.7775623211734342, 123.0390816101113245, 20.00000000000000000 ) ) ;
#5925 = VERTEX_POINT ( 'NONE', #13256 ) ;
#5926 = CARTESIAN_POINT ( 'NONE',  ( -17.29478376989774446, 30.34769730472564930, 61.62036986256358517 ) ) ;
#5927 = ORIENTED_EDGE ( 'NONE', *, *, #8313, .T. ) ;
#5928 = ORIENTED_EDGE ( 'NONE', *, *, #7644, .T. ) ;
#5929 = CYLINDRICAL_SURFACE ( 'NONE', #10045, 34.69999999999999574 ) ;
#5930 = DIRECTION ( 'NONE',  ( 0.000000000000000000, 0.000000000000000000, -1.000000000000000000 ) ) ;
#5931 = EDGE_LOOP ( 'NONE', ( #249, #13160, #8482, #298 ) ) ;
#5932 = VERTEX_POINT ( 'NONE', #1596 ) ;
#5933 = DIRECTION ( 'NONE',  ( 0.000000000000000000, -0.000000000000000000, -1.000000000000000000 ) ) ;
#5934 = DIRECTION ( 'NONE',  ( 0.000000000000000000, 0.000000000000000000, -1.000000000000000000 ) ) ;
#5935 = EDGE_CURVE ( 'NONE', #6071, #10428, #9232, .T. ) ;
#5936 = ORIENTED_EDGE ( 'NONE', *, *, #9864, .F. ) ;
#5937 = AXIS2_PLACEMENT_3D ( 'NONE', #11734, #2185, #6424 ) ;
#5938 = DIRECTION ( 'NONE',  ( 0.000000000000000000, 0.000000000000000000, 1.000000000000000000 ) ) ;
#5939 = DIRECTION ( 'NONE',  ( 1.000000000000000000, 0.000000000000000000, 0.000000000000000000 ) ) ;
#5940 = ORIENTED_EDGE ( 'NONE', *, *, #1407, .F. ) ;
#5941 = DIRECTION ( 'NONE',  ( -0.000000000000000000, -0.000000000000000000, 1.000000000000000000 ) ) ;
#5942 = CARTESIAN_POINT ( 'NONE',  ( 140.6356359024541973, 103.9054980190242361, 22.75000000000000000 ) ) ;
#5943 = EDGE_CURVE ( 'NONE', #11802, #12100, #3009, .T. ) ;
#5944 = ORIENTED_EDGE ( 'NONE', *, *, #11452, .T. ) ;
#5945 = AXIS2_PLACEMENT_3D ( 'NONE', #1097, #2170, #4389 ) ;
#5946 = ORIENTED_EDGE ( 'NONE', *, *, #6310, .T. ) ;
#5947 = CARTESIAN_POINT ( 'NONE',  ( -41.50918829505000218, -6.027090492554000534, 17.25000000000000000 ) ) ;
#5948 = EDGE_CURVE ( 'NONE', #7757, #8809, #10793, .T. ) ;
#5949 = CARTESIAN_POINT ( 'NONE',  ( -20.39103306562181928, 30.24295657639994772, 60.79987120566779879 ) ) ;
#5950 = CIRCLE ( 'NONE', #2872, 6.299999999999998046 ) ;
#5951 = PLANE ( 'NONE',  #9215 ) ;
#5952 = CIRCLE ( 'NONE', #13761, 0.9499999999999995115 ) ;
#5953 = DIRECTION ( 'NONE',  ( -0.000000000000000000, -0.000000000000000000, 1.000000000000000000 ) ) ;
#5954 = CARTESIAN_POINT ( 'NONE',  ( -18.05918829504999934, 10.97290950744599947, 58.54999999999999716 ) ) ;
#5955 = CIRCLE ( 'NONE', #2199, 10.74999999999999645 ) ;
#5956 = CARTESIAN_POINT ( 'NONE',  ( -24.37001676333060018, -4.028726038184999858, 62.14999999999999858 ) ) ;
#5957 = DIRECTION ( 'NONE',  ( 1.000000000000000000, 0.000000000000000000, 1.224646799147353207E-16 ) ) ;
#5958 = ORIENTED_EDGE ( 'NONE', *, *, #10035, .T. ) ;
#5959 = EDGE_CURVE ( 'NONE', #12260, #7947, #4773, .T. ) ;
#5960 = AXIS2_PLACEMENT_3D ( 'NONE', #7242, #11521, #8380 ) ;
#5961 = AXIS2_PLACEMENT_3D ( 'NONE', #4801, #3488, #12978 ) ;
#5962 = AXIS2_PLACEMENT_3D ( 'NONE', #4541, #12004, #2463 ) ;
#5963 = AXIS2_PLACEMENT_3D ( 'NONE', #10640, #5250, #5452 ) ;
#5964 = PLANE ( 'NONE',  #9952 ) ;
#5965 = ORIENTED_EDGE ( 'NONE', *, *, #6812, .F. ) ;
#5966 = ORIENTED_EDGE ( 'NONE', *, *, #6193, .F. ) ;
#5967 = LINE ( 'NONE', #9270, #3148 ) ;
#5968 = CARTESIAN_POINT ( 'NONE',  ( -18.05918829504999934, 10.97290950744599947, 63.64999999999999858 ) ) ;
#5969 = CARTESIAN_POINT ( 'NONE',  ( 140.6356359024541689, 85.03908161011133870, 0.7500000000000006661 ) ) ;
#5970 = DIRECTION ( 'NONE',  ( 0.000000000000000000, 0.000000000000000000, -1.000000000000000000 ) ) ;
#5971 = DIRECTION ( 'NONE',  ( 0.000000000000000000, 0.000000000000000000, -1.000000000000000000 ) ) ;
#5972 = CARTESIAN_POINT ( 'NONE',  ( 42.63563590245420443, 111.0390816101113387, 0.7500000000000000000 ) ) ;
#5973 = CYLINDRICAL_SURFACE ( 'NONE', #8667, 23.49999999999999645 ) ;
#5974 = CARTESIAN_POINT ( 'NONE',  ( -1.059188295049996231, 27.97290950744599769, 5.250000000000000000 ) ) ;
#5975 = DIRECTION ( 'NONE',  ( -1.000000000000000000, -0.000000000000000000, -0.000000000000000000 ) ) ;
#5976 = DIRECTION ( 'NONE',  ( 0.000000000000000000, 0.000000000000000000, 1.000000000000000000 ) ) ;
#5977 = CIRCLE ( 'NONE', #5526, 3.000000000000000000 ) ;
#5978 = AXIS2_PLACEMENT_3D ( 'NONE', #1418, #6852, #10225 ) ;
#5979 = CIRCLE ( 'NONE', #10240, 4.250000000000000000 ) ;
#5980 = AXIS2_PLACEMENT_3D ( 'NONE', #4406, #11300, #2663 ) ;
#5981 = ADVANCED_FACE ( 'NONE', ( #5704, #4806 ), #409, .F. ) ;
#5982 = PRODUCT_DEFINITION_CONTEXT ( 'detailed design', #5447, 'design' ) ;
#5983 = ORIENTED_EDGE ( 'NONE', *, *, #469, .F. ) ;
#5984 = EDGE_CURVE ( 'NONE', #12154, #7369, #12132, .T. ) ;
#5985 = VERTEX_POINT ( 'NONE', #11305 ) ;
#5986 = DIRECTION ( 'NONE',  ( -0.000000000000000000, -0.000000000000000000, 1.000000000000000000 ) ) ;
#5987 = PRODUCT_DEFINITION_FORMATION_WITH_SPECIFIED_SOURCE ( 'ANY', '', #12935, .NOT_KNOWN. ) ;
#5988 = AXIS2_PLACEMENT_3D ( 'NONE', #11886, #6567, #7446 ) ;
#5989 = AXIS2_PLACEMENT_3D ( 'NONE', #6673, #1498, #4791 ) ;
#5990 = ORIENTED_EDGE ( 'NONE', *, *, #5407, .T. ) ;
#5991 = DIRECTION ( 'NONE',  ( -1.000000000000000000, 0.000000000000000000, 0.000000000000000000 ) ) ;
#5992 = AXIS2_PLACEMENT_3D ( 'NONE', #10039, #4656, #4582 ) ;
#5993 = CARTESIAN_POINT ( 'NONE',  ( 140.6356359024541973, 94.90549801902425031, 22.75000000000000000 ) ) ;
#5994 = PRESENTATION_STYLE_ASSIGNMENT (( #11255 ) ) ;
#5995 = LINE ( 'NONE', #766, #2451 ) ;
#5996 = CARTESIAN_POINT ( 'NONE',  ( -10.47404583389237942, 25.90703532196704728, 57.35000000000000142 ) ) ;
#5997 = FACE_OUTER_BOUND ( 'NONE', #7534, .T. ) ;
#5998 = DIRECTION ( 'NONE',  ( -0.000000000000000000, -0.000000000000000000, -1.000000000000000000 ) ) ;
#5999 = AXIS2_PLACEMENT_3D ( 'NONE', #30, #5395, #9675 ) ;
#6000 = AXIS2_PLACEMENT_3D ( 'NONE', #4048, #8299, #12564 ) ;
#6001 = EDGE_CURVE ( 'NONE', #5058, #7296, #13457, .T. ) ;
#6002 = EDGE_CURVE ( 'NONE', #1128, #1821, #9277, .T. ) ;
#6003 = ORIENTED_EDGE ( 'NONE', *, *, #12890, .T. ) ;
#6004 = CARTESIAN_POINT ( 'NONE',  ( -15.56809582730673647, 30.22631440468149222, 60.65219431213508727 ) ) ;
#6005 = ORIENTED_EDGE ( 'NONE', *, *, #4255, .T. ) ;
#6006 = EDGE_LOOP ( 'NONE', ( #2133, #5045, #13485, #6581 ) ) ;
#6007 = CARTESIAN_POINT ( 'NONE',  ( 1.940811704950003991, -6.027090492554000534, 0.000000000000000000 ) ) ;
#6008 = DIRECTION ( 'NONE',  ( -1.000000000000000000, 1.239088197126291063E-16, 0.000000000000000000 ) ) ;
#6009 = ORIENTED_EDGE ( 'NONE', *, *, #8562, .T. ) ;
#6010 = CARTESIAN_POINT ( 'NONE',  ( 43.38563590245419732, 87.34974178189119698, 20.00000000000000000 ) ) ;
#6011 = DIRECTION ( 'NONE',  ( 0.000000000000000000, 0.000000000000000000, 1.000000000000000000 ) ) ;
#6012 = EDGE_LOOP ( 'NONE', ( #11748, #13213 ) ) ;
#6013 = DIRECTION ( 'NONE',  ( 0.000000000000000000, 0.000000000000000000, 1.000000000000000000 ) ) ;
#6014 = CIRCLE ( 'NONE', #13158, 2.000000000000001776 ) ;
#6015 = DIRECTION ( 'NONE',  ( 0.000000000000000000, 0.000000000000000000, -1.000000000000000000 ) ) ;
#6016 = AXIS2_PLACEMENT_3D ( 'NONE', #12873, #93, #1072 ) ;
#6017 = EDGE_LOOP ( 'NONE', ( #13644, #9966 ) ) ;
#6018 = CARTESIAN_POINT ( 'NONE',  ( -1.396365658198039927, 10.97290950744599947, 5.250000000000000000 ) ) ;
#6019 = DIRECTION ( 'NONE',  ( -0.000000000000000000, -0.000000000000000000, 1.000000000000000000 ) ) ;
#6020 = ORIENTED_EDGE ( 'NONE', *, *, #4436, .F. ) ;
#6021 = ORIENTED_EDGE ( 'NONE', *, *, #10161, .T. ) ;
#6022 = EDGE_CURVE ( 'NONE', #6726, #1270, #887, .T. ) ;
#6023 = AXIS2_PLACEMENT_3D ( 'NONE', #8007, #10380, #10186 ) ;
#6024 = CIRCLE ( 'NONE', #10724, 3.000000000000000000 ) ;
#6025 = CIRCLE ( 'NONE', #10, 1.000000000000000000 ) ;
#6026 = AXIS2_PLACEMENT_3D ( 'NONE', #6895, #11037, #545 ) ;
#6027 = EDGE_LOOP ( 'NONE', ( #6720, #1073, #4707, #8994 ) ) ;
#6028 = FACE_OUTER_BOUND ( 'NONE', #5679, .T. ) ;
#6029 = CARTESIAN_POINT ( 'NONE',  ( -0.04028432657539302714, 4.500000000000000000, 16.54539866546730309 ) ) ;
#6030 = EDGE_CURVE ( 'NONE', #721, #2952, #6657, .T. ) ;
#6031 = DIRECTION ( 'NONE',  ( 0.000000000000000000, 0.000000000000000000, -1.000000000000000000 ) ) ;
#6032 = DIRECTION ( 'NONE',  ( 0.000000000000000000, 0.000000000000000000, 1.000000000000000000 ) ) ;
#6033 = DIRECTION ( 'NONE',  ( 0.000000000000000000, 0.000000000000000000, -1.000000000000000000 ) ) ;
#6034 = FACE_BOUND ( 'NONE', #9286, .T. ) ;
#6035 = VECTOR ( 'NONE', #4192, 1000.000000000000000 ) ;
#6036 = APPLICATION_PROTOCOL_DEFINITION ( 'draft international standard', 'automotive_design', 1998, #3608 ) ;
#6037 = ORIENTED_EDGE ( 'NONE', *, *, #5657, .F. ) ;
#6038 = AXIS2_PLACEMENT_3D ( 'NONE', #11923, #5550, #9753 ) ;
#6039 = ORIENTED_EDGE ( 'NONE', *, *, #1566, .F. ) ;
#6040 = EDGE_CURVE ( 'NONE', #6370, #9883, #1415, .T. ) ;
#6041 = ORIENTED_EDGE ( 'NONE', *, *, #1348, .F. ) ;
#6042 =( BOUNDED_CURVE ( )  B_SPLINE_CURVE ( 3, ( #6696, #4750, #7942, #3643 ),
 .UNSPECIFIED., .F., .F. ) 
 B_SPLINE_CURVE_WITH_KNOTS ( ( 4, 4 ),
 ( 0.000000000000000000, 1.570796326794896558 ),
 .UNSPECIFIED. ) 
 CURVE ( )  GEOMETRIC_REPRESENTATION_ITEM ( )  RATIONAL_B_SPLINE_CURVE ( ( 1.000000000000000000, 0.8047378541243649375, 0.8047378541243649375, 1.000000000000000000 ) ) 
 REPRESENTATION_ITEM ( '' )  );
#6043 = CARTESIAN_POINT ( 'NONE',  ( 92.63563590245421153, 99.03908161011133870, 0.000000000000000000 ) ) ;
#6044 = CIRCLE ( 'NONE', #1142, 6.449999999999997513 ) ;
#6045 = EDGE_LOOP ( 'NONE', ( #2200, #2132, #6609, #11276 ) ) ;
#6046 = ORIENTED_EDGE ( 'NONE', *, *, #11878, .F. ) ;
#6047 = CARTESIAN_POINT ( 'NONE',  ( -7.999999999999998224, 2.000000000000000000, 0.000000000000000000 ) ) ;
#6048 = DIRECTION ( 'NONE',  ( -0.000000000000000000, -0.000000000000000000, -1.000000000000000000 ) ) ;
#6049 = EDGE_CURVE ( 'NONE', #3062, #8947, #1873, .T. ) ;
#6050 = CARTESIAN_POINT ( 'NONE',  ( -18.05918829504999934, 10.97290950744599947, 60.04999999999999716 ) ) ;
#6051 = CARTESIAN_POINT ( 'NONE',  ( -23.85417428574490373, 12.52794563810342154, 67.84999999999999432 ) ) ;
#6052 = VERTEX_POINT ( 'NONE', #8363 ) ;
#6053 = DIRECTION ( 'NONE',  ( 0.000000000000000000, 0.000000000000000000, -1.000000000000000000 ) ) ;
#6054 = DIRECTION ( 'NONE',  ( 1.000000000000000000, 0.000000000000000000, 0.000000000000000000 ) ) ;
#6055 = DIRECTION ( 'NONE',  ( 1.000000000000000000, 0.000000000000000000, 0.000000000000000000 ) ) ;
#6056 = DIRECTION ( 'NONE',  ( 0.000000000000000000, -1.000000000000000000, 0.000000000000000000 ) ) ;
#6057 = CARTESIAN_POINT ( 'NONE',  ( 4.500000000000002665, -4.336808689942017736E-16, 0.000000000000000000 ) ) ;
#6058 = VECTOR ( 'NONE', #6823, 1000.000000000000000 ) ;
#6059 = ORIENTED_EDGE ( 'NONE', *, *, #4646, .F. ) ;
#6060 = VERTEX_POINT ( 'NONE', #11441 ) ;
#6061 = LINE ( 'NONE', #10335, #5688 ) ;
#6062 = CYLINDRICAL_SURFACE ( 'NONE', #5046, 1.999999999999996669 ) ;
#6063 = ADVANCED_FACE ( 'NONE', ( #3842, #9216 ), #11506, .T. ) ;
#6064 = AXIS2_PLACEMENT_3D ( 'NONE', #457, #5751, #5546 ) ;
#6065 = CARTESIAN_POINT ( 'NONE',  ( -22.64501676333060232, -4.028726038184999858, 62.14999999999999858 ) ) ;
#6066 = CARTESIAN_POINT ( 'NONE',  ( -35.05918829505000645, 27.97290950744599769, 83.57661607529820458 ) ) ;
#6067 = FACE_OUTER_BOUND ( 'NONE', #1210, .T. ) ;
#6068 = DIRECTION ( 'NONE',  ( 0.000000000000000000, 3.387121092260455192E-15, 1.000000000000000000 ) ) ;
#6069 = CARTESIAN_POINT ( 'NONE',  ( -12.87735031270726083, -6.265087914666300328, 62.14999999999999858 ) ) ;
#6070 = VECTOR ( 'NONE', #7147, 1000.000000000000114 ) ;
#6071 = VERTEX_POINT ( 'NONE', #6184 ) ;
#6072 = VERTEX_POINT ( 'NONE', #10458 ) ;
#6073 = CARTESIAN_POINT ( 'NONE',  ( -15.68396707275562463, 30.23850757421161006, 60.76113458392060096 ) ) ;
#6074 = EDGE_LOOP ( 'NONE', ( #12843, #9521 ) ) ;
#6075 = CARTESIAN_POINT ( 'NONE',  ( -35.05918829505000645, 27.97290950744599769, 17.25000000000000000 ) ) ;
#6076 = CARTESIAN_POINT ( 'NONE',  ( -5.631644894983189431, 10.97290950744599947, 73.76763816269230745 ) ) ;
#6077 = VERTEX_POINT ( 'NONE', #1880 ) ;
#6078 = LINE ( 'NONE', #4080, #8652 ) ;
#6079 = PLANE ( 'NONE',  #5761 ) ;
#6080 = VERTEX_POINT ( 'NONE', #5010 ) ;
#6081 = CARTESIAN_POINT ( 'NONE',  ( -1.059188295049996231, -6.027090492554000534, 58.85000000000000142 ) ) ;
#6082 = CONICAL_SURFACE ( 'NONE', #64, 16.75000000000000355, 0.7853981633974447263 ) ;
#6083 = DIRECTION ( 'NONE',  ( 0.9496839325805432885, -0.3132098788326352912, 0.000000000000000000 ) ) ;
#6084 = EDGE_CURVE ( 'NONE', #1997, #54, #2487, .T. ) ;
#6085 = CARTESIAN_POINT ( 'NONE',  ( 2.877919977996279531E-15, 0.000000000000000000, 23.49999999999999645 ) ) ;
#6086 = EDGE_CURVE ( 'NONE', #12239, #4997, #11909, .T. ) ;
#6087 = DIRECTION ( 'NONE',  ( 0.000000000000000000, 0.000000000000000000, -1.000000000000000000 ) ) ;
#6088 = ADVANCED_FACE ( 'NONE', ( #4880 ), #5075, .F. ) ;
#6089 = EDGE_LOOP ( 'NONE', ( #844, #7489, #4036, #1503 ) ) ;
#6090 = VERTEX_POINT ( 'NONE', #7291 ) ;
#6091 = EDGE_LOOP ( 'NONE', ( #2204, #13020, #12895, #12427 ) ) ;
#6092 = ORIENTED_EDGE ( 'NONE', *, *, #9515, .T. ) ;
#6093 = ORIENTED_EDGE ( 'NONE', *, *, #3377, .F. ) ;
#6094 = LINE ( 'NONE', #5947, #6188 ) ;
#6095 = CARTESIAN_POINT ( 'NONE',  ( -19.65133266638497389, 30.30564942401206352, 61.31020756158706320 ) ) ;
#6096 = DIRECTION ( 'NONE',  ( 1.000000000000000000, 0.000000000000000000, 0.000000000000000000 ) ) ;
#6097 = CARTESIAN_POINT ( 'NONE',  ( 3.190811704950004657, -6.027090492554000534, 64.35000000000000853 ) ) ;
#6098 = FACE_OUTER_BOUND ( 'NONE', #12445, .T. ) ;
#6099 = EDGE_CURVE ( 'NONE', #10148, #2, #7648, .T. ) ;
#6100 = PLANE ( 'NONE',  #2033 ) ;
#6101 = DIRECTION ( 'NONE',  ( -1.000000000000000000, -6.780744947014009727E-15, 0.000000000000000000 ) ) ;
#6102 = ORIENTED_EDGE ( 'NONE', *, *, #1864, .F. ) ;
#6103 = ORIENTED_EDGE ( 'NONE', *, *, #712, .T. ) ;
#6104 = EDGE_CURVE ( 'NONE', #4904, #3980, #3443, .T. ) ;
#6105 = CARTESIAN_POINT ( 'NONE',  ( 116.7775623211734342, 112.2890816101113387, 0.000000000000000000 ) ) ;
#6106 = ORIENTED_EDGE ( 'NONE', *, *, #7825, .T. ) ;
#6107 = VERTEX_POINT ( 'NONE', #12360 ) ;
#6108 = DIRECTION ( 'NONE',  ( -1.000000000000000000, 0.000000000000000000, 0.000000000000000000 ) ) ;
#6109 = CARTESIAN_POINT ( 'NONE',  ( -16.55918829504999579, 21.47290950744600124, 57.35000000000000142 ) ) ;
#6110 = DIRECTION ( 'NONE',  ( -0.000000000000000000, -0.000000000000000000, -1.000000000000000000 ) ) ;
#6111 = CARTESIAN_POINT ( 'NONE',  ( 8.500000000000003553, 2.499999999999999556, -65.00000000000000000 ) ) ;
#6112 = DIRECTION ( 'NONE',  ( 0.000000000000000000, 0.000000000000000000, 1.000000000000000000 ) ) ;
#6113 = CYLINDRICAL_SURFACE ( 'NONE', #419, 6.000000000000002665 ) ;
#6114 = LINE ( 'NONE', #7226, #11184 ) ;
#6115 = EDGE_CURVE ( 'NONE', #3543, #4612, #4326, .T. ) ;
#6116 = CARTESIAN_POINT ( 'NONE',  ( 50.63563590245420443, 94.90549801902425031, 22.75000000000000000 ) ) ;
#6117 = DIRECTION ( 'NONE',  ( 0.6615960714621574867, -0.7498604124941119498, 0.000000000000000000 ) ) ;
#6118 = UNCERTAINTY_MEASURE_WITH_UNIT (LENGTH_MEASURE( 1.000000000000000082E-05 ), #9964, 'distance_accuracy_value', 'NONE');
#6119 = ADVANCED_FACE ( 'NONE', ( #2871 ), #13243, .T. ) ;
#6120 = CIRCLE ( 'NONE', #10826, 4.250000000000000000 ) ;
#6121 = ORIENTED_EDGE ( 'NONE', *, *, #5287, .F. ) ;
#6122 = CARTESIAN_POINT ( 'NONE',  ( -32.35918829505000360, 27.97290950744599769, 64.85000000000000853 ) ) ;
#6123 = ORIENTED_EDGE ( 'NONE', *, *, #11591, .T. ) ;
#6124 = CLOSED_SHELL ( 'NONE', ( #7365, #7182, #5849, #3477, #8176, #4346, #1319, #4585, #239, #11017, #10364, #9928, #35, #8817, #10475, #421, #12249 ) ) ;
#6125 = VERTEX_POINT ( 'NONE', #3015 ) ;
#6126 = VERTEX_POINT ( 'NONE', #7094 ) ;
#6127 = CARTESIAN_POINT ( 'NONE',  ( -18.88016301897669891, 16.91647750172969822, 67.84999999999999432 ) ) ;
#6128 = CARTESIAN_POINT ( 'NONE',  ( 43.38563590245419732, 87.03908161011136713, 20.00000000000000000 ) ) ;
#6129 = DIRECTION ( 'NONE',  ( 0.000000000000000000, 1.000000000000000000, 0.000000000000000000 ) ) ;
#6130 = ORIENTED_EDGE ( 'NONE', *, *, #1950, .T. ) ;
#6131 = DIRECTION ( 'NONE',  ( 1.000000000000000000, 0.000000000000000000, 0.000000000000000000 ) ) ;
#6132 = EDGE_CURVE ( 'NONE', #1301, #12138, #7874, .T. ) ;
#6133 = VECTOR ( 'NONE', #8712, 1000.000000000000000 ) ;
#6134 = CARTESIAN_POINT ( 'NONE',  ( -16.04064420431702942, 4.500000000000000000, -7.307586582922255047 ) ) ;
#6135 = EDGE_CURVE ( 'NONE', #2697, #7324, #7786, .T. ) ;
#6136 = EDGE_LOOP ( 'NONE', ( #10815, #7491, #2844, #2397 ) ) ;
#6137 = AXIS2_PLACEMENT_3D ( 'NONE', #6043, #10318, #8077 ) ;
#6138 = CARTESIAN_POINT ( 'NONE',  ( -14.51101483699455841, 30.08769857173034623, 58.98207106897987728 ) ) ;
#6139 = EDGE_LOOP ( 'NONE', ( #3250, #1928, #3450, #7118 ) ) ;
#6140 = CARTESIAN_POINT ( 'NONE',  ( -15.54512322349380149, 8.123439939968370993, 27.09999999999999787 ) ) ;
#6141 = LINE ( 'NONE', #7188, #2270 ) ;
#6142 = CARTESIAN_POINT ( 'NONE',  ( 82.99521369064696330, 82.14063840035363739, 10.00000000000000000 ) ) ;
#6143 = ORIENTED_EDGE ( 'NONE', *, *, #1052, .T. ) ;
#6144 = ORIENTED_EDGE ( 'NONE', *, *, #11475, .F. ) ;
#6145 = DIRECTION ( 'NONE',  ( 1.000000000000000000, 0.000000000000000000, 0.000000000000000000 ) ) ;
#6146 = DIRECTION ( 'NONE',  ( 0.000000000000000000, 0.000000000000000000, -1.000000000000000000 ) ) ;
#6147 = ORIENTED_EDGE ( 'NONE', *, *, #8978, .T. ) ;
#6148 = LINE ( 'NONE', #1771, #9607 ) ;
#6149 = DIRECTION ( 'NONE',  ( -1.000000000000000000, -0.000000000000000000, -0.000000000000000000 ) ) ;
#6150 = DIRECTION ( 'NONE',  ( -0.000000000000000000, -0.000000000000000000, -1.000000000000000000 ) ) ;
#6151 = AXIS2_PLACEMENT_3D ( 'NONE', #10485, #7187, #7249 ) ;
#6152 = LINE ( 'NONE', #10424, #1804 ) ;
#6153 = ORIENTED_EDGE ( 'NONE', *, *, #11445, .F. ) ;
#6154 = VERTEX_POINT ( 'NONE', #5346 ) ;
#6155 = ORIENTED_EDGE ( 'NONE', *, *, #9908, .F. ) ;
#6156 = ADVANCED_FACE ( 'NONE', ( #5275 ), #1783, .F. ) ;
#6157 = ORIENTED_EDGE ( 'NONE', *, *, #736, .F. ) ;
#6158 = ORIENTED_EDGE ( 'NONE', *, *, #10479, .T. ) ;
#6159 = CIRCLE ( 'NONE', #10407, 2.700000000000000178 ) ;
#6160 = LINE ( 'NONE', #8272, #3987 ) ;
#6161 = CYLINDRICAL_SURFACE ( 'NONE', #1599, 2.000000000000001776 ) ;
#6162 = DIRECTION ( 'NONE',  ( -1.000000000000000000, 0.000000000000000000, 0.000000000000000000 ) ) ;
#6163 = CARTESIAN_POINT ( 'NONE',  ( 44.63563590245420443, 108.9054980190242503, 20.00000000000000000 ) ) ;
#6164 = DIRECTION ( 'NONE',  ( 1.000000000000000000, 0.000000000000000000, 0.000000000000000000 ) ) ;
#6165 = FACE_BOUND ( 'NONE', #5100, .T. ) ;
#6166 = DIRECTION ( 'NONE',  ( 0.000000000000000000, 0.000000000000000000, 1.000000000000000000 ) ) ;
#6167 =( REPRESENTATION_RELATIONSHIP ('NONE','NONE', #11848, #5062 ) REPRESENTATION_RELATIONSHIP_WITH_TRANSFORMATION ( #10792 )SHAPE_REPRESENTATION_RELATIONSHIP( ) );
#6168 = ORIENTED_EDGE ( 'NONE', *, *, #1866, .F. ) ;
#6169 = ORIENTED_EDGE ( 'NONE', *, *, #279, .T. ) ;
#6170 = MECHANICAL_DESIGN_GEOMETRIC_PRESENTATION_REPRESENTATION (  '', ( #4629 ), #2637 ) ;
#6171 = EDGE_CURVE ( 'NONE', #2279, #1108, #653, .T. ) ;
#6172 = DIRECTION ( 'NONE',  ( 1.000000000000000000, 0.000000000000000000, 0.000000000000000000 ) ) ;
#6173 = CARTESIAN_POINT ( 'NONE',  ( -35.05918829505000645, -6.027090492554000534, 17.25000000000000000 ) ) ;
#6174 = ORIENTED_EDGE ( 'NONE', *, *, #10960, .F. ) ;
#6175 = CARTESIAN_POINT ( 'NONE',  ( 98.27605811426136029, 115.9375248198690826, 10.00000000000000000 ) ) ;
#6176 = CARTESIAN_POINT ( 'NONE',  ( -1.059188295049996231, 27.97290950744599769, 64.35000000000000853 ) ) ;
#6177 = CIRCLE ( 'NONE', #10000, 3.000000000000001332 ) ;
#6178 = LINE ( 'NONE', #5140, #8500 ) ;
#6179 = DIRECTION ( 'NONE',  ( 0.000000000000000000, 0.000000000000000000, 1.000000000000000000 ) ) ;
#6180 = VERTEX_POINT ( 'NONE', #9486 ) ;
#6181 = CARTESIAN_POINT ( 'NONE',  ( -18.05918829504999934, 10.97290950744599947, 60.40999999999999659 ) ) ;
#6182 = CARTESIAN_POINT ( 'NONE',  ( 134.8856359024541973, 104.1554980190242361, 23.00000000000000000 ) ) ;
#6183 = CARTESIAN_POINT ( 'NONE',  ( -35.05918829505000645, 27.97290950744599769, 5.250000000000000000 ) ) ;
#6184 = CARTESIAN_POINT ( 'NONE',  ( -1.059188295049996231, 10.97290950744599947, 63.54999999999999716 ) ) ;
#6185 = FACE_OUTER_BOUND ( 'NONE', #1553, .T. ) ;
#6186 = CIRCLE ( 'NONE', #13548, 8.395833332999998788 ) ;
#6187 = ORIENTED_EDGE ( 'NONE', *, *, #2034, .F. ) ;
#6188 = VECTOR ( 'NONE', #1704, 1000.000000000000000 ) ;
#6189 = ORIENTED_EDGE ( 'NONE', *, *, #10641, .F. ) ;
#6190 = ADVANCED_FACE ( 'NONE', ( #9549, #3413, #13729, #2161, #12824, #11579 ), #11716, .F. ) ;
#6191 = CARTESIAN_POINT ( 'NONE',  ( -28.87730642030695094, 29.81324547859994922, 5.250000000000000000 ) ) ;
#6192 = ORIENTED_EDGE ( 'NONE', *, *, #13085, .F. ) ;
#6193 = EDGE_CURVE ( 'NONE', #4071, #4170, #6341, .T. ) ;
#6194 = DIRECTION ( 'NONE',  ( 1.000000000000000000, 0.000000000000000000, 0.000000000000000000 ) ) ;
#6195 = ORIENTED_EDGE ( 'NONE', *, *, #7907, .F. ) ;
#6196 = CARTESIAN_POINT ( 'NONE',  ( -32.05918829504999934, -6.027090492554000534, 0.000000000000000000 ) ) ;
#6197 = CIRCLE ( 'NONE', #8685, 24.04163056034261459 ) ;
#6198 = AXIS2_PLACEMENT_3D ( 'NONE', #4544, #2113, #6351 ) ;
#6199 = FILL_AREA_STYLE_COLOUR ( '', #1608 ) ;
#6200 = CONICAL_SURFACE ( 'NONE', #178, 6.145833333000002341, 0.2014252309328122270 ) ;
#6201 = CIRCLE ( 'NONE', #10904, 2.700000000000001066 ) ;
#6202 = DIRECTION ( 'NONE',  ( -1.000000000000000000, 0.000000000000000000, 0.000000000000000000 ) ) ;
#6203 = AXIS2_PLACEMENT_3D ( 'NONE', #2595, #3637, #12211 ) ;
#6204 = ADVANCED_FACE ( 'NONE', ( #12697 ), #4322, .T. ) ;
#6205 = DIRECTION ( 'NONE',  ( 1.000000000000000000, 0.000000000000000000, 0.000000000000000000 ) ) ;
#6206 = VECTOR ( 'NONE', #7228, 1000.000000000000000 ) ;
#6207 = VECTOR ( 'NONE', #4405, 1000.000000000000114 ) ;
#6208 = VECTOR ( 'NONE', #12193, 1000.000000000000000 ) ;
#6209 = VERTEX_POINT ( 'NONE', #10664 ) ;
#6210 = EDGE_CURVE ( 'NONE', #4357, #8162, #8561, .T. ) ;
#6211 = VECTOR ( 'NONE', #5341, 1000.000000000000227 ) ;
#6212 = CARTESIAN_POINT ( 'NONE',  ( -15.33453732926608915, 30.19994085548103513, 60.40352641156652425 ) ) ;
#6213 = EDGE_LOOP ( 'NONE', ( #4739, #6238, #4134, #7824 ) ) ;
#6214 = EDGE_LOOP ( 'NONE', ( #2373, #2709, #4293, #12257 ) ) ;
#6215 = ORIENTED_EDGE ( 'NONE', *, *, #5747, .T. ) ;
#6216 = CARTESIAN_POINT ( 'NONE',  ( -1.059188295049996231, -6.027090492554000534, 83.57661607529820458 ) ) ;
#6217 = SURFACE_STYLE_USAGE ( .BOTH. , #4003 ) ;
#6218 = DIRECTION ( 'NONE',  ( -0.000000000000000000, -0.000000000000000000, 1.000000000000000000 ) ) ;
#6219 = ORIENTED_EDGE ( 'NONE', *, *, #8920, .T. ) ;
#6220 = DIRECTION ( 'NONE',  ( 0.000000000000000000, 0.000000000000000000, -1.000000000000000000 ) ) ;
#6221 = DIRECTION ( 'NONE',  ( 0.000000000000000000, 0.000000000000000000, -1.000000000000000000 ) ) ;
#6222 = ORIENTED_EDGE ( 'NONE', *, *, #12611, .T. ) ;
#6223 = EDGE_CURVE ( 'NONE', #8617, #7248, #1090, .T. ) ;
#6224 = DIRECTION ( 'NONE',  ( 0.000000000000000000, 0.000000000000000000, -1.000000000000000000 ) ) ;
#6225 =( GEOMETRIC_REPRESENTATION_CONTEXT ( 3 ) GLOBAL_UNCERTAINTY_ASSIGNED_CONTEXT ( ( #12421 ) ) GLOBAL_UNIT_ASSIGNED_CONTEXT ( ( #5756, #13034, #3748 ) ) REPRESENTATION_CONTEXT ( 'NONE', 'WORKASPACE' ) );
#6226 = CARTESIAN_POINT ( 'NONE',  ( 8.157609394192110841, 24.73469418910620021, 17.25000000000000000 ) ) ;
#6227 = CARTESIAN_POINT ( 'NONE',  ( 10.81426999815522549, -15.06602133594279991, 0.000000000000000000 ) ) ;
#6228 = DIRECTION ( 'NONE',  ( 0.000000000000000000, -1.000000000000000000, 0.000000000000000000 ) ) ;
#6229 = CIRCLE ( 'NONE', #1547, 18.50000000000000000 ) ;
#6230 = ORIENTED_EDGE ( 'NONE', *, *, #5164, .F. ) ;
#6231 = ORIENTED_EDGE ( 'NONE', *, *, #3526, .T. ) ;
#6232 = ORIENTED_EDGE ( 'NONE', *, *, #7120, .T. ) ;
#6233 = ORIENTED_EDGE ( 'NONE', *, *, #13648, .F. ) ;
#6234 = VECTOR ( 'NONE', #10954, 1000.000000000000000 ) ;
#6235 = ORIENTED_EDGE ( 'NONE', *, *, #112, .T. ) ;
#6236 = LINE ( 'NONE', #7406, #2437 ) ;
#6237 = LINE ( 'NONE', #10512, #11342 ) ;
#6238 = ORIENTED_EDGE ( 'NONE', *, *, #3847, .T. ) ;
#6239 = EDGE_CURVE ( 'NONE', #217, #3941, #10688, .T. ) ;
#6240 = CARTESIAN_POINT ( 'NONE',  ( -18.05918829504999934, 10.97290950744599947, 30.59999999999999787 ) ) ;
#6241 = CARTESIAN_POINT ( 'NONE',  ( -18.93268260677970716, 26.94904914358915704, 56.13056362116011400 ) ) ;
#6242 = DIRECTION ( 'NONE',  ( 0.3132098788326365124, -0.9496839325805429555, 0.000000000000000000 ) ) ;
#6243 = CARTESIAN_POINT ( 'NONE',  ( -18.05918829504999934, 10.97290950744599947, 11.50000000000000000 ) ) ;
#6244 = DIRECTION ( 'NONE',  ( -0.000000000000000000, -0.000000000000000000, 1.000000000000000000 ) ) ;
#6245 = SHAPE_DEFINITION_REPRESENTATION ( #6352, #5062 ) ;
#6246 = EDGE_LOOP ( 'NONE', ( #8633, #1976 ) ) ;
#6247 = ADVANCED_BREP_SHAPE_REPRESENTATION ( '', ( #348, #6434 ), #6225 ) ;
#6248 = VECTOR ( 'NONE', #10122, 1000.000000000000000 ) ;
#6249 = VECTOR ( 'NONE', #2609, 1000.000000000000000 ) ;
#6250 = VECTOR ( 'NONE', #8264, 1000.000000000000000 ) ;
#6251 = AXIS2_PLACEMENT_3D ( 'NONE', #3764, #9138, #2665 ) ;
#6252 = ORIENTED_EDGE ( 'NONE', *, *, #13701, .T. ) ;
#6253 = ORIENTED_EDGE ( 'NONE', *, *, #2617, .T. ) ;
#6254 = FACE_OUTER_BOUND ( 'NONE', #4479, .T. ) ;
#6255 = CARTESIAN_POINT ( 'NONE',  ( 9.640422211807132769, 16.89844320975774750, 7.000000000000000000 ) ) ;
#6256 = ORIENTED_EDGE ( 'NONE', *, *, #928, .T. ) ;
#6257 = DIRECTION ( 'NONE',  ( -0.000000000000000000, 1.000000000000000000, -0.000000000000000000 ) ) ;
#6258 = DIRECTION ( 'NONE',  ( 0.000000000000000000, 0.000000000000000000, -1.000000000000000000 ) ) ;
#6259 = DIRECTION ( 'NONE',  ( 0.000000000000000000, 0.000000000000000000, -1.000000000000000000 ) ) ;
#6260 = AXIS2_PLACEMENT_3D ( 'NONE', #12654, #11604, #7053 ) ;
#6261 = AXIS2_PLACEMENT_3D ( 'NONE', #8376, #10547, #977 ) ;
#6262 = VECTOR ( 'NONE', #11888, 1000.000000000000000 ) ;
#6263 = CARTESIAN_POINT ( 'NONE',  ( -18.05918829504999934, 7.130333642789880244, 5.250000000000000000 ) ) ;
#6264 = DIRECTION ( 'NONE',  ( 1.000000000000000000, 0.000000000000000000, 0.000000000000000000 ) ) ;
#6265 = AXIS2_PLACEMENT_3D ( 'NONE', #9705, #3493, #12904 ) ;
#6266 = DIRECTION ( 'NONE',  ( 1.000000000000000000, 0.000000000000000000, 0.000000000000000000 ) ) ;
#6267 = DIRECTION ( 'NONE',  ( 0.000000000000000000, 0.000000000000000000, -1.000000000000000000 ) ) ;
#6268 = CARTESIAN_POINT ( 'NONE',  ( 50.63563590245420443, 94.90549801902425031, 20.00000000000000000 ) ) ;
#6269 = LINE ( 'NONE', #5216, #6206 ) ;
#6270 = ADVANCED_FACE ( 'NONE', ( #11777 ), #2097, .T. ) ;
#6271 = EDGE_CURVE ( 'NONE', #3389, #13286, #10597, .T. ) ;
#6272 = ORIENTED_EDGE ( 'NONE', *, *, #8868, .F. ) ;
#6273 = VECTOR ( 'NONE', #2188, 1000.000000000000114 ) ;
#6274 = AXIS2_PLACEMENT_3D ( 'NONE', #3071, #6110, #7355 ) ;
#6275 = AXIS2_PLACEMENT_3D ( 'NONE', #5150, #11504, #9484 ) ;
#6276 = EDGE_LOOP ( 'NONE', ( #2131, #5886, #3097, #1094, #8797, #3384, #5048, #13122, #11894, #5284, #3096, #4531, #2317, #5103, #2525 ) ) ;
#6277 = EDGE_CURVE ( 'NONE', #4755, #8888, #6543, .T. ) ;
#6278 = DIRECTION ( 'NONE',  ( 0.000000000000000000, 0.000000000000000000, -1.000000000000000000 ) ) ;
#6279 = ORIENTED_EDGE ( 'NONE', *, *, #8487, .T. ) ;
#6280 = ORIENTED_EDGE ( 'NONE', *, *, #5690, .F. ) ;
#6281 = CARTESIAN_POINT ( 'NONE',  ( 4.500000000000002665, -4.336808689942017736E-16, -65.00000000000000000 ) ) ;
#6282 = ORIENTED_EDGE ( 'NONE', *, *, #11055, .T. ) ;
#6283 = DIRECTION ( 'NONE',  ( 0.000000000000000000, 0.000000000000000000, 1.000000000000000000 ) ) ;
#6284 = CARTESIAN_POINT ( 'NONE',  ( -7.241070169793059286, 29.81324547859994922, 5.250000000000000000 ) ) ;
#6285 = CARTESIAN_POINT ( 'NONE',  ( -1.859188294733151059, 2.872909506853357442, 63.35000000001166143 ) ) ;
#6286 = AXIS2_PLACEMENT_3D ( 'NONE', #3285, #12708, #978 ) ;
#6287 = AXIS2_PLACEMENT_3D ( 'NONE', #6791, #2564, #10016 ) ;
#6288 = CARTESIAN_POINT ( 'NONE',  ( -18.05918829504999934, 10.97290950744599947, 62.14999999999999858 ) ) ;
#6289 = AXIS2_PLACEMENT_3D ( 'NONE', #5531, #3317, #12808 ) ;
#6290 = EDGE_CURVE ( 'NONE', #11290, #642, #966, .T. ) ;
#6291 = EDGE_CURVE ( 'NONE', #510, #13024, #8498, .T. ) ;
#6292 = ORIENTED_EDGE ( 'NONE', *, *, #10486, .T. ) ;
#6293 = CIRCLE ( 'NONE', #12988, 1.999999999999991340 ) ;
#6294 = CARTESIAN_POINT ( 'NONE',  ( -14.73910058758217723, 30.12180271180697133, 55.18720206871329736 ) ) ;
#6295 = VERTEX_POINT ( 'NONE', #1223 ) ;
#6296 = ORIENTED_EDGE ( 'NONE', *, *, #5596, .T. ) ;
#6297 = ORIENTED_EDGE ( 'NONE', *, *, #75, .F. ) ;
#6298 = LINE ( 'NONE', #10559, #7259 ) ;
#6299 = LINE ( 'NONE', #5304, #13174 ) ;
#6300 = CARTESIAN_POINT ( 'NONE',  ( -16.08092853089235774, 4.500000000000000000, 7.237812082545088899 ) ) ;
#6301 = ORIENTED_EDGE ( 'NONE', *, *, #6551, .T. ) ;
#6302 = ORIENTED_EDGE ( 'NONE', *, *, #6399, .T. ) ;
#6303 = FACE_OUTER_BOUND ( 'NONE', #13766, .T. ) ;
#6304 = DIRECTION ( 'NONE',  ( 0.000000000000000000, -1.000000000000000000, 0.000000000000000000 ) ) ;
#6305 = FACE_OUTER_BOUND ( 'NONE', #11841, .T. ) ;
#6306 = EDGE_CURVE ( 'NONE', #6072, #912, #4690, .T. ) ;
#6307 = DIRECTION ( 'NONE',  ( -0.000000000000000000, -0.000000000000000000, -1.000000000000000000 ) ) ;
#6308 = VECTOR ( 'NONE', #2576, 1000.000000000000000 ) ;
#6309 = ORIENTED_EDGE ( 'NONE', *, *, #7902, .T. ) ;
#6310 = EDGE_CURVE ( 'NONE', #6705, #13129, #9367, .T. ) ;
#6311 = VERTEX_POINT ( 'NONE', #1296 ) ;
#6312 = EDGE_LOOP ( 'NONE', ( #4719, #9330, #652, #11418, #330, #2019, #4624, #2713, #4771, #13164, #6798, #8580, #104 ) ) ;
#6313 = ORIENTED_EDGE ( 'NONE', *, *, #10960, .T. ) ;
#6314 = VECTOR ( 'NONE', #13153, 1000.000000000000000 ) ;
#6315 = ORIENTED_EDGE ( 'NONE', *, *, #11973, .F. ) ;
#6316 = CARTESIAN_POINT ( 'NONE',  ( 18.45469220996244886, 1.832421873814834123, -3.000000000000000000 ) ) ;
#6317 = DIRECTION ( 'NONE',  ( 0.000000000000000000, 0.000000000000000000, -1.000000000000000000 ) ) ;
#6318 = VERTEX_POINT ( 'NONE', #8839 ) ;
#6319 = DIRECTION ( 'NONE',  ( 2.267612386897784912E-16, -1.000000000000000000, 0.000000000000000000 ) ) ;
#6320 = CARTESIAN_POINT ( 'NONE',  ( -35.05918829505000645, 27.97290950744599769, 68.85549045786049760 ) ) ;
#6321 = DIRECTION ( 'NONE',  ( 0.000000000000000000, 0.000000000000000000, -1.000000000000000000 ) ) ;
#6322 = CARTESIAN_POINT ( 'NONE',  ( -35.05918829505000645, -6.027090492554000534, 10.00000000000000000 ) ) ;
#6323 = EDGE_CURVE ( 'NONE', #10024, #3793, #7114, .T. ) ;
#6324 = FACE_OUTER_BOUND ( 'NONE', #6342, .T. ) ;
#6325 = APPLICATION_PROTOCOL_DEFINITION ( 'draft international standard', 'automotive_design', 1998, #4054 ) ;
#6326 = EDGE_CURVE ( 'NONE', #6125, #2972, #11925, .T. ) ;
#6327 = AXIS2_PLACEMENT_3D ( 'NONE', #10298, #7904, #783 ) ;
#6328 = EDGE_CURVE ( 'NONE', #1042, #642, #3578, .T. ) ;
#6329 = VERTEX_POINT ( 'NONE', #5627 ) ;
#6330 = ORIENTED_EDGE ( 'NONE', *, *, #13427, .F. ) ;
#6331 = CARTESIAN_POINT ( 'NONE',  ( -10.25088531517539714, 30.80589556422609832, 83.57661607529820458 ) ) ;
#6332 = ORIENTED_EDGE ( 'NONE', *, *, #7232, .T. ) ;
#6333 = DIRECTION ( 'NONE',  ( 0.000000000000000000, -1.000000000000000000, 0.000000000000000000 ) ) ;
#6334 = CARTESIAN_POINT ( 'NONE',  ( -18.05918829504999934, 30.47290950744599769, 61.89660000000000650 ) ) ;
#6335 = SURFACE_SIDE_STYLE ('',( #9746 ) ) ;
#6336 = CARTESIAN_POINT ( 'NONE',  ( -20.13390280776154384, 30.26743272311685118, 53.69271067728588775 ) ) ;
#6337 = SURFACE_STYLE_FILL_AREA ( #5339 ) ;
#6338 = CARTESIAN_POINT ( 'NONE',  ( 140.6356359024541973, 94.90549801902425031, 23.00000000000000000 ) ) ;
#6339 = LINE ( 'NONE', #10594, #2220 ) ;
#6340 = DIRECTION ( 'NONE',  ( 0.000000000000000000, 0.000000000000000000, -1.000000000000000000 ) ) ;
#6341 = LINE ( 'NONE', #6268, #12042 ) ;
#6342 = EDGE_LOOP ( 'NONE', ( #4954, #2828, #4131, #9025 ) ) ;
#6343 = VERTEX_POINT ( 'NONE', #4793 ) ;
#6344 = CARTESIAN_POINT ( 'NONE',  ( 140.5320825118609207, 94.80194462843097369, 23.00000000000000000 ) ) ;
#6345 = EDGE_CURVE ( 'NONE', #2105, #9316, #12489, .T. ) ;
#6346 = EDGE_LOOP ( 'NONE', ( #6810, #10541, #1096, #4275 ) ) ;
#6347 = CARTESIAN_POINT ( 'NONE',  ( -13.29473957835121389, 8.508638270346013499, 68.48645984990002944 ) ) ;
#6348 = DIRECTION ( 'NONE',  ( 0.000000000000000000, 1.000000000000000000, 0.000000000000000000 ) ) ;
#6349 = FILL_AREA_STYLE ('',( #193 ) ) ;
#6350 = DIRECTION ( 'NONE',  ( 0.000000000000000000, 0.000000000000000000, -1.000000000000000000 ) ) ;
#6351 = DIRECTION ( 'NONE',  ( 1.000000000000000000, 0.000000000000000000, 0.000000000000000000 ) ) ;
#6352 = PRODUCT_DEFINITION_SHAPE ( 'NONE', 'NONE',  #11074 ) ;
#6353 = EDGE_LOOP ( 'NONE', ( #11064, #1671, #12134, #1196 ) ) ;
#6354 = CARTESIAN_POINT ( 'NONE',  ( -15.32570436422911975, 30.19895062898915938, 54.30601320233879648 ) ) ;
#6355 = EDGE_LOOP ( 'NONE', ( #365, #2603, #3661, #5691 ) ) ;
#6356 = ORIENTED_EDGE ( 'NONE', *, *, #111, .T. ) ;
#6357 = VERTEX_POINT ( 'NONE', #1374 ) ;
#6358 = EDGE_CURVE ( 'NONE', #2858, #3543, #12923, .T. ) ;
#6359 = ORIENTED_EDGE ( 'NONE', *, *, #11254, .T. ) ;
#6360 = DIRECTION ( 'NONE',  ( 0.4528443260392608916, 0.8915896008669279560, 0.000000000000000000 ) ) ;
#6361 = VECTOR ( 'NONE', #7754, 1000.000000000000000 ) ;
#6362 = CARTESIAN_POINT ( 'NONE',  ( -18.05918829504999934, 10.97290950744599947, 53.85000000000000142 ) ) ;
#6363 = ORIENTED_EDGE ( 'NONE', *, *, #7319, .F. ) ;
#6364 = FACE_OUTER_BOUND ( 'NONE', #11533, .T. ) ;
#6365 = FACE_OUTER_BOUND ( 'NONE', #4830, .T. ) ;
#6366 = CARTESIAN_POINT ( 'NONE',  ( 82.99521369064696330, 82.14063840035363739, 10.00000000000000000 ) ) ;
#6367 = FACE_BOUND ( 'NONE', #804, .T. ) ;
#6368 = AXIS2_PLACEMENT_3D ( 'NONE', #8230, #6278, #9147 ) ;
#6369 = ORIENTED_EDGE ( 'NONE', *, *, #10248, .F. ) ;
#6370 = VERTEX_POINT ( 'NONE', #3683 ) ;
#6371 = ORIENTED_EDGE ( 'NONE', *, *, #5599, .T. ) ;
#6372 = EDGE_CURVE ( 'NONE', #8976, #9897, #6458, .T. ) ;
#6373 = ORIENTED_EDGE ( 'NONE', *, *, #12028, .T. ) ;
#6374 = EDGE_LOOP ( 'NONE', ( #6232, #10165, #7493, #6737 ) ) ;
#6375 = LINE ( 'NONE', #2801, #8431 ) ;
#6376 = DIRECTION ( 'NONE',  ( -1.000000000000000000, 0.000000000000000000, 0.000000000000000000 ) ) ;
#6377 = VECTOR ( 'NONE', #12552, 1000.000000000000000 ) ;
#6378 = ADVANCED_FACE ( 'NONE', ( #3623 ), #1575, .T. ) ;
#6379 = LINE ( 'NONE', #8681, #7367 ) ;
#6380 = CARTESIAN_POINT ( 'NONE',  ( -19.02868427256591133, 26.94368128781859539, 56.20497232447349489 ) ) ;
#6381 = CARTESIAN_POINT ( 'NONE',  ( 50.38563590245420443, 94.90549801902425031, 22.75000000000000000 ) ) ;
#6382 = DIRECTION ( 'NONE',  ( 0.4528443260392608916, 0.8915896008669279560, 0.000000000000000000 ) ) ;
#6383 = ADVANCED_FACE ( 'NONE', ( #2581 ), #11083, .T. ) ;
#6384 = DIRECTION ( 'NONE',  ( -1.000000000000000000, 0.000000000000000000, 0.000000000000000000 ) ) ;
#6385 = AXIS2_PLACEMENT_3D ( 'NONE', #3612, #13089, #11913 ) ;
#6386 = EDGE_LOOP ( 'NONE', ( #7203, #9146, #8387, #6520 ) ) ;
#6387 = EDGE_CURVE ( 'NONE', #6644, #13079, #5755, .T. ) ;
#6388 = DIRECTION ( 'NONE',  ( 1.000000000000000000, 0.000000000000000000, 0.000000000000000000 ) ) ;
#6389 = LINE ( 'NONE', #5406, #2689 ) ;
#6390 = FACE_OUTER_BOUND ( 'NONE', #9785, .T. ) ;
#6391 = CARTESIAN_POINT ( 'NONE',  ( -1.559188295050000006, 10.97290950744599947, 57.35000000000000142 ) ) ;
#6392 = CARTESIAN_POINT ( 'NONE',  ( -20.76349711708835954, 30.20233709048880755, 54.27308111598625118 ) ) ;
#6393 = DIRECTION ( 'NONE',  ( 0.000000000000000000, 0.000000000000000000, -1.000000000000000000 ) ) ;
#6394 = ORIENTED_EDGE ( 'NONE', *, *, #1917, .F. ) ;
#6395 = CARTESIAN_POINT ( 'NONE',  ( -1.059188295049996231, 27.97290950744599769, 17.25000000000000000 ) ) ;
#6396 = CARTESIAN_POINT ( 'NONE',  ( -18.05918829488915023, 18.13901823688300396, 61.72253826514069885 ) ) ;
#6397 = DIRECTION ( 'NONE',  ( 0.000000000000000000, 0.000000000000000000, -1.000000000000000000 ) ) ;
#6398 = CIRCLE ( 'NONE', #1713, 6.449999999999997513 ) ;
#6399 = EDGE_CURVE ( 'NONE', #8485, #87, #6905, .T. ) ;
#6400 = DIRECTION ( 'NONE',  ( 0.7071067811865567876, 0.7071067811865382469, 0.000000000000000000 ) ) ;
#6401 = VERTEX_POINT ( 'NONE', #264 ) ;
#6402 = CIRCLE ( 'NONE', #5945, 10.74999999999999645 ) ;
#6403 = DIRECTION ( 'NONE',  ( 0.000000000000000000, 0.000000000000000000, -1.000000000000000000 ) ) ;
#6404 = ORIENTED_EDGE ( 'NONE', *, *, #8140, .F. ) ;
#6405 = ORIENTED_EDGE ( 'NONE', *, *, #1353, .T. ) ;
#6406 = ORIENTED_EDGE ( 'NONE', *, *, #5444, .F. ) ;
#6407 = DIRECTION ( 'NONE',  ( 0.000000000000000000, 0.000000000000000000, 1.000000000000000000 ) ) ;
#6408 = CARTESIAN_POINT ( 'NONE',  ( -38.38077571930826082, 22.44393519180575680, 5.250000000000000000 ) ) ;
#6409 = LINE ( 'NONE', #1100, #3844 ) ;
#6410 = ORIENTED_EDGE ( 'NONE', *, *, #5444, .T. ) ;
#6411 = LINE ( 'NONE', #5290, #1992 ) ;
#6412 = EDGE_CURVE ( 'NONE', #6850, #12924, #9907, .T. ) ;
#6413 = CARTESIAN_POINT ( 'NONE',  ( 7.347880794884120722E-16, 8.500000000000000000, -6.000000000000000888 ) ) ;
#6414 = AXIS2_PLACEMENT_3D ( 'NONE', #12357, #542, #3838 ) ;
#6415 = STYLED_ITEM ( 'NONE', ( #6537 ), #9635 ) ;
#6416 = UNCERTAINTY_MEASURE_WITH_UNIT (LENGTH_MEASURE( 1.000000000000000082E-05 ), #4949, 'distance_accuracy_value', 'NONE');
#6417 = ORIENTED_EDGE ( 'NONE', *, *, #5061, .T. ) ;
#6418 = CARTESIAN_POINT ( 'NONE',  ( -15.23092771910337717, 30.18746625253793425, 54.42100116539269550 ) ) ;
#6419 = AXIS2_PLACEMENT_3D ( 'NONE', #6288, #5227, #10342 ) ;
#6420 = AXIS2_PLACEMENT_3D ( 'NONE', #13110, #3633, #10889 ) ;
#6421 = VECTOR ( 'NONE', #3986, 1000.000000000000000 ) ;
#6422 = EDGE_LOOP ( 'NONE', ( #553, #9166, #10928, #4832 ) ) ;
#6423 = ORIENTED_EDGE ( 'NONE', *, *, #2306, .T. ) ;
#6424 = DIRECTION ( 'NONE',  ( -1.000000000000000000, 0.000000000000000000, 0.000000000000000000 ) ) ;
#6425 = AXIS2_PLACEMENT_3D ( 'NONE', #3192, #11694, #2005 ) ;
#6426 = CARTESIAN_POINT ( 'NONE',  ( -35.05918829505000645, 27.97290950744599769, 64.85000000000000853 ) ) ;
#6427 = SURFACE_SIDE_STYLE ('',( #7518 ) ) ;
#6428 = ORIENTED_EDGE ( 'NONE', *, *, #12512, .T. ) ;
#6429 = ORIENTED_EDGE ( 'NONE', *, *, #7619, .F. ) ;
#6430 = DIRECTION ( 'NONE',  ( 0.000000000000000000, 0.000000000000000000, 1.000000000000000000 ) ) ;
#6431 = DIRECTION ( 'NONE',  ( 0.000000000000000000, 0.000000000000000000, -1.000000000000000000 ) ) ;
#6432 = CARTESIAN_POINT ( 'NONE',  ( -1.899121662050003101, 19.05294282444601706, 63.34900083300006202 ) ) ;
#6433 = PLANE ( 'NONE',  #11389 ) ;
#6434 = AXIS2_PLACEMENT_3D ( 'NONE', #11654, #12825, #11856 ) ;
#6435 = EDGE_CURVE ( 'NONE', #1261, #4307, #8918, .T. ) ;
#6436 = AXIS2_PLACEMENT_3D ( 'NONE', #5549, #4657, #10040 ) ;
#6437 = ADVANCED_FACE ( 'NONE', ( #11147 ), #5829, .F. ) ;
#6438 = AXIS2_PLACEMENT_3D ( 'NONE', #13493, #1626, #6011 ) ;
#6439 = VERTEX_POINT ( 'NONE', #13307 ) ;
#6440 = DIRECTION ( 'NONE',  ( 0.000000000000000000, 0.000000000000000000, 1.000000000000000000 ) ) ;
#6441 = ORIENTED_EDGE ( 'NONE', *, *, #5217, .T. ) ;
#6442 = ORIENTED_EDGE ( 'NONE', *, *, #7709, .F. ) ;
#6443 = VERTEX_POINT ( 'NONE', #10878 ) ;
#6444 = ORIENTED_EDGE ( 'NONE', *, *, #928, .F. ) ;
#6445 = AXIS2_PLACEMENT_3D ( 'NONE', #12472, #5957, #1710 ) ;
#6446 = LINE ( 'NONE', #10713, #853 ) ;
#6447 = CARTESIAN_POINT ( 'NONE',  ( -10.25088531517539714, 30.80589556422609832, 17.25000000000000000 ) ) ;
#6448 = AXIS2_PLACEMENT_3D ( 'NONE', #13590, #10455, #884 ) ;
#6449 = ORIENTED_EDGE ( 'NONE', *, *, #1777, .T. ) ;
#6450 = DIRECTION ( 'NONE',  ( -0.7071067811865525687, -0.7071067811865425767, 0.000000000000000000 ) ) ;
#6451 = LINE ( 'NONE', #4230, #3644 ) ;
#6452 = CARTESIAN_POINT ( 'NONE',  ( 43.38563590245419732, 85.03908161011133870, 0.7500000000000006661 ) ) ;
#6453 = CARTESIAN_POINT ( 'NONE',  ( -18.05918829504999934, 10.97290950744599947, 61.85000000000000142 ) ) ;
#6454 = CARTESIAN_POINT ( 'NONE',  ( 12.81426999815521839, -15.06602133594279991, -3.000000000000000000 ) ) ;
#6455 = CONTEXT_DEPENDENT_SHAPE_REPRESENTATION ( #7322, #10956 ) ;
#6456 = ADVANCED_FACE ( 'NONE', ( #3478 ), #7706, .F. ) ;
#6457 = AXIS2_PLACEMENT_3D ( 'NONE', #3802, #8972, #2706 ) ;
#6458 = CIRCLE ( 'NONE', #890, 17.00000000000000000 ) ;
#6459 = ORIENTED_EDGE ( 'NONE', *, *, #12551, .T. ) ;
#6460 = ADVANCED_FACE ( 'NONE', ( #2515, #1438, #6034, #12471, #10311, #7996, #9326, #2998, #6165, #3889, #1926, #731 ), #6100, .T. ) ;
#6461 = DIRECTION ( 'NONE',  ( 1.000000000000000000, 0.000000000000000000, 0.000000000000000000 ) ) ;
#6462 = DIRECTION ( 'NONE',  ( 1.000000000000000000, 0.000000000000000000, -0.000000000000000000 ) ) ;
#6463 = FACE_OUTER_BOUND ( 'NONE', #8842, .T. ) ;
#6464 = CYLINDRICAL_SURFACE ( 'NONE', #13763, 0.7499999999999924505 ) ;
#6465 = DIRECTION ( 'NONE',  ( -0.000000000000000000, 1.000000000000000000, -0.000000000000000000 ) ) ;
#6466 = DIRECTION ( 'NONE',  ( 0.000000000000000000, -1.000000000000000000, 0.000000000000000000 ) ) ;
#6467 = ORIENTED_EDGE ( 'NONE', *, *, #8159, .F. ) ;
#6468 = DIRECTION ( 'NONE',  ( -1.000000000000000000, 0.000000000000000000, 0.000000000000000000 ) ) ;
#6469 = DIRECTION ( 'NONE',  ( 1.000000000000000000, -9.130123557772674004E-16, 0.000000000000000000 ) ) ;
#6470 = CARTESIAN_POINT ( 'NONE',  ( -18.05918829309690210, 18.59099508048574734, 61.65955166400529919 ) ) ;
#6471 = DIRECTION ( 'NONE',  ( 0.000000000000000000, 0.000000000000000000, -1.000000000000000000 ) ) ;
#6472 = AXIS2_PLACEMENT_3D ( 'NONE', #5095, #2759, #13336 ) ;
#6473 = AXIS2_PLACEMENT_3D ( 'NONE', #6587, #2567, #5735 ) ;
#6474 = EDGE_CURVE ( 'NONE', #2380, #11544, #9822, .T. ) ;
#6475 = EDGE_CURVE ( 'NONE', #12138, #7324, #2471, .T. ) ;
#6476 = AXIS2_PLACEMENT_3D ( 'NONE', #667, #12409, #4871 ) ;
#6477 = DIRECTION ( 'NONE',  ( 0.2878798879079290662, 0.9576665234506832602, 0.000000000000000000 ) ) ;
#6478 = AXIS2_PLACEMENT_3D ( 'NONE', #3582, #6708, #356 ) ;
#6479 = AXIS2_PLACEMENT_3D ( 'NONE', #5720, #5442, #5653 ) ;
#6480 = AXIS2_PLACEMENT_3D ( 'NONE', #1693, #5938, #10228 ) ;
#6481 = EDGE_LOOP ( 'NONE', ( #2694, #9726, #2423, #11821 ) ) ;
#6482 = ORIENTED_EDGE ( 'NONE', *, *, #5536, .T. ) ;
#6483 = CARTESIAN_POINT ( 'NONE',  ( -10.78334210919089919, 29.19143287883919768, 64.85000000000000853 ) ) ;
#6484 = CARTESIAN_POINT ( 'NONE',  ( -43.05918829505002066, 32.97290950744599769, 0.000000000000000000 ) ) ;
#6485 = CYLINDRICAL_SURFACE ( 'NONE', #8067, 16.72262947720610171 ) ;
#6486 = CARTESIAN_POINT ( 'NONE',  ( -19.91165729514404603, 13.07251866242952154, 23.90000000000000213 ) ) ;
#6487 = CARTESIAN_POINT ( 'NONE',  ( -18.05918829504999934, 10.97290950744599947, 63.64999999999999858 ) ) ;
#6488 = DIRECTION ( 'NONE',  ( 0.000000000000000000, 0.000000000000000000, 1.000000000000000000 ) ) ;
#6489 = LINE ( 'NONE', #8794, #11551 ) ;
#6490 = ADVANCED_FACE ( 'NONE', ( #4861 ), #4995, .F. ) ;
#6491 = VECTOR ( 'NONE', #10946, 1000.000000000000000 ) ;
#6492 = AXIS2_PLACEMENT_3D ( 'NONE', #12899, #3426, #1308 ) ;
#6493 = VECTOR ( 'NONE', #12150, 1000.000000000000000 ) ;
#6494 = VERTEX_POINT ( 'NONE', #10373 ) ;
#6495 = ADVANCED_FACE ( 'NONE', ( #12402 ), #1862, .F. ) ;
#6496 = CARTESIAN_POINT ( 'NONE',  ( -17.20179490422193780, 30.34444651895395850, 53.10284867194972946 ) ) ;
#6497 = ORIENTED_EDGE ( 'NONE', *, *, #636, .F. ) ;
#6498 = ORIENTED_EDGE ( 'NONE', *, *, #13216, .T. ) ;
#6499 = ORIENTED_EDGE ( 'NONE', *, *, #5181, .T. ) ;
#6500 = CARTESIAN_POINT ( 'NONE',  ( -10.79835982676942052, -4.028726038184999858, 63.45000000000000284 ) ) ;
#6501 = STYLED_ITEM ( 'NONE', ( #210 ), #4352 ) ;
#6502 = CARTESIAN_POINT ( 'NONE',  ( 5.999999999999999112, -12.00000000000000178, 0.000000000000000000 ) ) ;
#6503 = VECTOR ( 'NONE', #5195, 1000.000000000000000 ) ;
#6504 = DIRECTION ( 'NONE',  ( 0.000000000000000000, 0.000000000000000000, 1.000000000000000000 ) ) ;
#6505 = VECTOR ( 'NONE', #6033, 1000.000000000000000 ) ;
#6506 = VERTEX_POINT ( 'NONE', #2720 ) ;
#6507 = LINE ( 'NONE', #10991, #7772 ) ;
#6508 = CARTESIAN_POINT ( 'NONE',  ( 185.2712718049083946, 90.15549801902423610, 23.00000000000000000 ) ) ;
#6509 = LINE ( 'NONE', #10566, #450 ) ;
#6510 = CYLINDRICAL_SURFACE ( 'NONE', #12060, 2.000000000000001776 ) ;
#6511 = VECTOR ( 'NONE', #12777, 1000.000000000000114 ) ;
#6512 = EDGE_LOOP ( 'NONE', ( #1839, #3482, #6757, #12637 ) ) ;
#6513 = LINE ( 'NONE', #9083, #560 ) ;
#6514 = ORIENTED_EDGE ( 'NONE', *, *, #4643, .T. ) ;
#6515 = ORIENTED_EDGE ( 'NONE', *, *, #11608, .F. ) ;
#6516 = ORIENTED_EDGE ( 'NONE', *, *, #8878, .T. ) ;
#6517 = CARTESIAN_POINT ( 'NONE',  ( -25.05563313235659706, -2.802149825948039741, 58.54999999999999716 ) ) ;
#6518 = ADVANCED_FACE ( 'NONE', ( #11222 ), #6950, .F. ) ;
#6519 = DIRECTION ( 'NONE',  ( -1.000000000000000000, 0.000000000000000000, 0.000000000000000000 ) ) ;
#6520 = ORIENTED_EDGE ( 'NONE', *, *, #714, .F. ) ;
#6521 = CARTESIAN_POINT ( 'NONE',  ( -38.63164489498320364, 10.97290950744599947, 73.76763816269230745 ) ) ;
#6522 = CIRCLE ( 'NONE', #13434, 1.725000000000000755 ) ;
#6523 = CARTESIAN_POINT ( 'NONE',  ( -17.28440556981917808, 26.95410257713844615, 56.06541086284084230 ) ) ;
#6524 = DIRECTION ( 'NONE',  ( 1.000000000000000000, 0.000000000000000000, 0.000000000000000000 ) ) ;
#6525 = DIRECTION ( 'NONE',  ( 1.000000000000000000, 0.000000000000000000, 0.000000000000000000 ) ) ;
#6526 = DIRECTION ( 'NONE',  ( 0.000000000000000000, -1.000000000000000000, 0.000000000000000000 ) ) ;
#6527 = ITEM_DEFINED_TRANSFORMATION ( 'NONE', 'NONE', #9569,  #6434 ) ;
#6528 = AXIS2_PLACEMENT_3D ( 'NONE', #3391, #4715, #8757 ) ;
#6529 = PRODUCT_DEFINITION_SHAPE ( 'NONE', 'NONE',  #4332 ) ;
#6530 = ORIENTED_EDGE ( 'NONE', *, *, #11721, .F. ) ;
#6531 = VERTEX_POINT ( 'NONE', #8278 ) ;
#6532 = CYLINDRICAL_SURFACE ( 'NONE', #1930, 6.049999999999999822 ) ;
#6533 = ORIENTED_EDGE ( 'NONE', *, *, #1664, .F. ) ;
#6534 = DIRECTION ( 'NONE',  ( 0.000000000000000000, 0.000000000000000000, -1.000000000000000000 ) ) ;
#6535 = CARTESIAN_POINT ( 'NONE',  ( -41.50918829505000218, -6.027090492554000534, 83.57661607529820458 ) ) ;
#6536 = EDGE_CURVE ( 'NONE', #3266, #10507, #10932, .T. ) ;
#6537 = PRESENTATION_STYLE_ASSIGNMENT (( #1289 ) ) ;
#6538 = CARTESIAN_POINT ( 'NONE',  ( -20.27573349293325933, 30.25428168448397415, 53.80284863901545833 ) ) ;
#6539 = CARTESIAN_POINT ( 'NONE',  ( -1.059188295049996231, -6.027090492554000534, 10.00000000000000000 ) ) ;
#6540 = CARTESIAN_POINT ( 'NONE',  ( -1.059188295049996231, -6.027090492554000534, 64.35000000000000853 ) ) ;
#6541 = CYLINDRICAL_SURFACE ( 'NONE', #6662, 1.999999999999996669 ) ;
#6542 = VECTOR ( 'NONE', #6083, 1000.000000000000114 ) ;
#6543 = LINE ( 'NONE', #9692, #7331 ) ;
#6544 = ADVANCED_FACE ( 'NONE', ( #3819 ), #11488, .T. ) ;
#6545 = ORIENTED_EDGE ( 'NONE', *, *, #1790, .T. ) ;
#6546 = AXIS2_PLACEMENT_3D ( 'NONE', #12078, #8860, #7872 ) ;
#6547 = FACE_BOUND ( 'NONE', #7647, .T. ) ;
#6548 = VERTEX_POINT ( 'NONE', #596 ) ;
#6549 = EDGE_LOOP ( 'NONE', ( #8649, #1737, #9353, #3851 ) ) ;
#6550 = DIRECTION ( 'NONE',  ( -1.000000000000000000, 0.000000000000000000, 0.000000000000000000 ) ) ;
#6551 = EDGE_CURVE ( 'NONE', #707, #9911, #2256, .T. ) ;
#6552 = FACE_OUTER_BOUND ( 'NONE', #7756, .T. ) ;
#6553 = DIRECTION ( 'NONE',  ( 0.000000000000000000, 0.000000000000000000, 1.000000000000000000 ) ) ;
#6554 = DIRECTION ( 'NONE',  ( -0.000000000000000000, 1.000000000000000000, -0.000000000000000000 ) ) ;
#6555 = CARTESIAN_POINT ( 'NONE',  ( 140.6356359024541973, 94.90549801902425031, 20.00000000000000000 ) ) ;
#6556 = CYLINDRICAL_SURFACE ( 'NONE', #7866, 6.000000000000000888 ) ;
#6557 = DIRECTION ( 'NONE',  ( 1.000000000000000000, 0.000000000000000000, 0.000000000000000000 ) ) ;
#6558 = ADVANCED_FACE ( 'NONE', ( #2790 ), #227, .T. ) ;
#6559 = ORIENTED_EDGE ( 'NONE', *, *, #8350, .T. ) ;
#6560 = PRESENTATION_LAYER_ASSIGNMENT (  '', '', ( #12596 ) ) ;
#6561 = CARTESIAN_POINT ( 'NONE',  ( -17.24607760227289077, 30.34604302011652521, 53.09143874144074005 ) ) ;
#6562 = ADVANCED_FACE ( 'NONE', ( #3953 ), #8203, .F. ) ;
#6563 = LINE ( 'NONE', #10831, #2171 ) ;
#6564 = LINE ( 'NONE', #10989, #13602 ) ;
#6565 = DIRECTION ( 'NONE',  ( 0.000000000000000000, 0.000000000000000000, 1.000000000000000000 ) ) ;
#6566 = EDGE_LOOP ( 'NONE', ( #1869, #12682, #4022, #7958, #5383, #5661, #3050, #4235, #3577, #3944, #10250, #5514, #7775, #8060, #3368, #1479 ) ) ;
#6567 = DIRECTION ( 'NONE',  ( 0.3132098788326395100, 0.9496839325805419563, 0.000000000000000000 ) ) ;
#6568 = DIRECTION ( 'NONE',  ( -0.7071067811865500152, -0.7071067811865451302, -0.000000000000000000 ) ) ;
#6569 = EDGE_CURVE ( 'NONE', #10012, #13212, #11426, .T. ) ;
#6570 = DIRECTION ( 'NONE',  ( -0.000000000000000000, -0.000000000000000000, 1.000000000000000000 ) ) ;
#6571 = VERTEX_POINT ( 'NONE', #9196 ) ;
#6572 = ORIENTED_EDGE ( 'NONE', *, *, #10585, .F. ) ;
#6573 = ORIENTED_EDGE ( 'NONE', *, *, #8428, .T. ) ;
#6574 = CIRCLE ( 'NONE', #10601, 8.300000000000000711 ) ;
#6575 = CARTESIAN_POINT ( 'NONE',  ( -35.05918829505000645, 27.97290950744599769, 68.85549045786049760 ) ) ;
#6576 = ORIENTED_EDGE ( 'NONE', *, *, #4696, .T. ) ;
#6577 = VERTEX_POINT ( 'NONE', #13447 ) ;
#6578 = ORIENTED_EDGE ( 'NONE', *, *, #6536, .F. ) ;
#6579 = DIRECTION ( 'NONE',  ( 1.000000000000000000, 0.000000000000000000, 0.000000000000000000 ) ) ;
#6580 = DIRECTION ( 'NONE',  ( 0.000000000000000000, 0.000000000000000000, -1.000000000000000000 ) ) ;
#6581 = ORIENTED_EDGE ( 'NONE', *, *, #3803, .T. ) ;
#6582 = DIRECTION ( 'NONE',  ( 0.000000000000000000, 0.000000000000000000, -1.000000000000000000 ) ) ;
#6583 = LINE ( 'NONE', #9945, #8111 ) ;
#6584 = CARTESIAN_POINT ( 'NONE',  ( -34.68447646404997897, 19.28555359244599288, 63.26601075299999621 ) ) ;
#6585 = CARTESIAN_POINT ( 'NONE',  ( -18.05918829504999934, 10.97290950744599947, 64.85000000000000853 ) ) ;
#6586 = AXIS2_PLACEMENT_3D ( 'NONE', #757, #8369, #12634 ) ;
#6587 = CARTESIAN_POINT ( 'NONE',  ( -18.05918829504999934, 10.97290950744599947, 61.65000000000000568 ) ) ;
#6588 = ADVANCED_FACE ( 'NONE', ( #6324 ), #5134, .T. ) ;
#6589 = VERTEX_POINT ( 'NONE', #3060 ) ;
#6590 = CIRCLE ( 'NONE', #12833, 6.000000000000000888 ) ;
#6591 = DIRECTION ( 'NONE',  ( 0.000000000000000000, 0.000000000000000000, -1.000000000000000000 ) ) ;
#6592 = DIRECTION ( 'NONE',  ( 1.000000000000000000, -0.000000000000000000, -0.000000000000000000 ) ) ;
#6593 = VERTEX_POINT ( 'NONE', #2215 ) ;
#6594 = FACE_BOUND ( 'NONE', #1948, .T. ) ;
#6595 = CYLINDRICAL_SURFACE ( 'NONE', #841, 0.2500000000000002220 ) ;
#6596 = CARTESIAN_POINT ( 'NONE',  ( -19.29163931862649406, 30.32761401381639033, 53.22486482497648552 ) ) ;
#6597 = LINE ( 'NONE', #12191, #11215 ) ;
#6598 = CARTESIAN_POINT ( 'NONE',  ( -18.05918829505001355, 18.23680593644599668, 62.03182374100007479 ) ) ;
#6599 = DIRECTION ( 'NONE',  ( 1.000000000000000000, 0.000000000000000000, 0.000000000000000000 ) ) ;
#6600 = LINE ( 'NONE', #11715, #7591 ) ;
#6601 = DIRECTION ( 'NONE',  ( -1.000000000000000000, 0.000000000000000000, 0.000000000000000000 ) ) ;
#6602 = VECTOR ( 'NONE', #10651, 1000.000000000000000 ) ;
#6603 = EDGE_CURVE ( 'NONE', #6784, #1834, #9841, .T. ) ;
#6604 = EDGE_CURVE ( 'NONE', #7369, #1, #2012, .T. ) ;
#6605 = VERTEX_POINT ( 'NONE', #8475 ) ;
#6606 = ORIENTED_EDGE ( 'NONE', *, *, #5268, .F. ) ;
#6607 = EDGE_LOOP ( 'NONE', ( #6429, #5345 ) ) ;
#6608 = LINE ( 'NONE', #13803, #2601 ) ;
#6609 = ORIENTED_EDGE ( 'NONE', *, *, #11835, .T. ) ;
#6610 = LINE ( 'NONE', #2589, #896 ) ;
#6611 = ORIENTED_EDGE ( 'NONE', *, *, #2777, .T. ) ;
#6612 = FACE_OUTER_BOUND ( 'NONE', #5049, .T. ) ;
#6613 = AXIS2_PLACEMENT_3D ( 'NONE', #9766, #3282, #11934 ) ;
#6614 = DIRECTION ( 'NONE',  ( 1.000000000000000000, -0.000000000000000000, -0.000000000000000000 ) ) ;
#6615 = DIRECTION ( 'NONE',  ( -8.673617379884027583E-16, 1.000000000000000000, -0.000000000000000000 ) ) ;
#6616 = DIRECTION ( 'NONE',  ( 0.000000000000000000, 0.000000000000000000, 1.000000000000000000 ) ) ;
#6617 = CARTESIAN_POINT ( 'NONE',  ( -24.35918829505000005, 10.97290950744599947, 61.86500000000000199 ) ) ;
#6618 = DIRECTION ( 'NONE',  ( -0.000000000000000000, -0.000000000000000000, -1.000000000000000000 ) ) ;
#6619 = CARTESIAN_POINT ( 'NONE',  ( -35.05918829505000645, 27.97290950744599769, 64.85000000000000853 ) ) ;
#6620 = CARTESIAN_POINT ( 'NONE',  ( -23.05918829504999934, 10.97290950744599947, 118.8499999999999943 ) ) ;
#6621 =( REPRESENTATION_RELATIONSHIP ('NONE','NONE', #11848, #10413 ) REPRESENTATION_RELATIONSHIP_WITH_TRANSFORMATION ( #10584 )SHAPE_REPRESENTATION_RELATIONSHIP( ) );
#6622 = ORIENTED_EDGE ( 'NONE', *, *, #12098, .T. ) ;
#6623 = ADVANCED_FACE ( 'NONE', ( #11632 ), #7335, .T. ) ;
#6624 = ORIENTED_EDGE ( 'NONE', *, *, #6983, .F. ) ;
#6625 = CARTESIAN_POINT ( 'NONE',  ( -15.52422514065462877, 30.22157476238875162, 54.09163654685160338 ) ) ;
#6626 = ORIENTED_EDGE ( 'NONE', *, *, #1375, .T. ) ;
#6627 = ADVANCED_FACE ( 'NONE', ( #9602 ), #10583, .F. ) ;
#6628 = DIRECTION ( 'NONE',  ( -1.000000000000000000, 0.000000000000000000, 0.000000000000000000 ) ) ;
#6629 = CIRCLE ( 'NONE', #613, 23.22993838181875148 ) ;
#6630 = ORIENTED_EDGE ( 'NONE', *, *, #3969, .T. ) ;
#6631 = CARTESIAN_POINT ( 'NONE',  ( 62.16596598834396303, 68.56941169600129626, 19.25000000000000000 ) ) ;
#6632 = DIRECTION ( 'NONE',  ( -0.000000000000000000, -0.000000000000000000, 1.000000000000000000 ) ) ;
#6633 = DIRECTION ( 'NONE',  ( 0.000000000000000000, 0.000000000000000000, 1.000000000000000000 ) ) ;
#6634 = EDGE_CURVE ( 'NONE', #952, #2401, #11597, .T. ) ;
#6635 = CIRCLE ( 'NONE', #10232, 5.500000000000000888 ) ;
#6636 = ORIENTED_EDGE ( 'NONE', *, *, #5865, .F. ) ;
#6637 = AXIS2_PLACEMENT_3D ( 'NONE', #13767, #13385, #1655 ) ;
#6638 = EDGE_LOOP ( 'NONE', ( #1144, #316, #10083, #13022 ) ) ;
#6639 = AXIS2_PLACEMENT_3D ( 'NONE', #10432, #791, #5050 ) ;
#6640 = ADVANCED_FACE ( 'NONE', ( #4305 ), #2145, .F. ) ;
#6641 = DIRECTION ( 'NONE',  ( -0.9496839325805422893, 0.3132098788326386218, 0.000000000000000000 ) ) ;
#6642 = ORIENTED_EDGE ( 'NONE', *, *, #12957, .T. ) ;
#6643 = EDGE_LOOP ( 'NONE', ( #3673, #4295, #6970, #7592, #12836, #9302 ) ) ;
#6644 = VERTEX_POINT ( 'NONE', #1140 ) ;
#6645 = EDGE_CURVE ( 'NONE', #10203, #12272, #13714, .T. ) ;
#6646 = ORIENTED_EDGE ( 'NONE', *, *, #2071, .F. ) ;
#6647 = CARTESIAN_POINT ( 'NONE',  ( -18.05918829504999934, 30.36027202460864771, 52.99086025162979752 ) ) ;
#6648 = DIRECTION ( 'NONE',  ( 0.000000000000000000, 0.000000000000000000, -1.000000000000000000 ) ) ;
#6649 = ORIENTED_EDGE ( 'NONE', *, *, #4373, .T. ) ;
#6650 = CARTESIAN_POINT ( 'NONE',  ( 81.82136590429890077, 114.1051029460540605, 10.00000000000000000 ) ) ;
#6651 = DIRECTION ( 'NONE',  ( 1.000000000000000000, 0.000000000000000000, 0.000000000000000000 ) ) ;
#6652 = VECTOR ( 'NONE', #8966, 1000.000000000000000 ) ;
#6653 = PLANE ( 'NONE',  #7746 ) ;
#6654 = FACE_OUTER_BOUND ( 'NONE', #8138, .T. ) ;
#6655 = AXIS2_PLACEMENT_3D ( 'NONE', #7393, #6221, #6304 ) ;
#6656 = CARTESIAN_POINT ( 'NONE',  ( 3.190811704950004657, -6.027090492554000534, 58.85000000000000142 ) ) ;
#6657 =( BOUNDED_CURVE ( )  B_SPLINE_CURVE ( 3, ( #8222, #2807, #5910, #12486 ),
 .UNSPECIFIED., .F., .F. ) 
 B_SPLINE_CURVE_WITH_KNOTS ( ( 4, 4 ),
 ( 1.570796326794896558, 3.141592653589793116 ),
 .UNSPECIFIED. ) 
 CURVE ( )  GEOMETRIC_REPRESENTATION_ITEM ( )  RATIONAL_B_SPLINE_CURVE ( ( 1.000000000000000000, 0.8047378541243649375, 0.8047378541243649375, 1.000000000000000000 ) ) 
 REPRESENTATION_ITEM ( '' )  );
#6658 = EDGE_LOOP ( 'NONE', ( #7475, #11723, #13662, #838 ) ) ;
#6659 =( GEOMETRIC_REPRESENTATION_CONTEXT ( 3 ) GLOBAL_UNCERTAINTY_ASSIGNED_CONTEXT ( ( #11444 ) ) GLOBAL_UNIT_ASSIGNED_CONTEXT ( ( #4996, #13580, #5056 ) ) REPRESENTATION_CONTEXT ( 'NONE', 'WORKASPACE' ) );
#6660 = VERTEX_POINT ( 'NONE', #3260 ) ;
#6661 = CIRCLE ( 'NONE', #9797, 1.999999999999994893 ) ;
#6662 = AXIS2_PLACEMENT_3D ( 'NONE', #12694, #9623, #3334 ) ;
#6663 = EDGE_LOOP ( 'NONE', ( #9935, #6559, #7991, #8249, #6313, #415, #12155, #2360 ) ) ;
#6664 = AXIS2_PLACEMENT_3D ( 'NONE', #10325, #12414, #3012 ) ;
#6665 = EDGE_CURVE ( 'NONE', #3112, #10847, #7469, .T. ) ;
#6666 = DIRECTION ( 'NONE',  ( -0.000000000000000000, 1.000000000000000000, -0.000000000000000000 ) ) ;
#6667 = CARTESIAN_POINT ( 'NONE',  ( 109.0903281124166710, 100.8715034839261762, 20.00000000000000000 ) ) ;
#6668 = DIRECTION ( 'NONE',  ( 0.000000000000000000, 0.000000000000000000, 1.000000000000000000 ) ) ;
#6669 = DIRECTION ( 'NONE',  ( 1.000000000000000000, 0.000000000000000000, 0.000000000000000000 ) ) ;
#6670 = CARTESIAN_POINT ( 'NONE',  ( -20.65862537727294068, 30.21441468393235041, 60.54187128424251085 ) ) ;
#6671 = SURFACE_SIDE_STYLE ('',( #3542 ) ) ;
#6672 = CARTESIAN_POINT ( 'NONE',  ( -23.85417428574490373, 12.52794563810342154, 68.84999999999999432 ) ) ;
#6673 = CARTESIAN_POINT ( 'NONE',  ( 116.7775623211734342, 123.0390816101113245, 19.25000000000000000 ) ) ;
#6674 = CARTESIAN_POINT ( 'NONE',  ( -12.00000000000000000, -2.500000000000000444, -65.00000000000000000 ) ) ;
#6675 = DIRECTION ( 'NONE',  ( -1.000000000000000000, 0.000000000000000000, 0.000000000000000000 ) ) ;
#6676 = AXIS2_PLACEMENT_3D ( 'NONE', #6453, #11971, #6382 ) ;
#6677 = AXIS2_PLACEMENT_3D ( 'NONE', #4659, #6809, #6675 ) ;
#6678 = VERTEX_POINT ( 'NONE', #4369 ) ;
#6679 = EDGE_LOOP ( 'NONE', ( #9415, #7349, #10705, #7750 ) ) ;
#6680 = ORIENTED_EDGE ( 'NONE', *, *, #10227, .F. ) ;
#6681 = CARTESIAN_POINT ( 'NONE',  ( 6.940811704950001548, 32.97290950744599769, 10.00000000000000000 ) ) ;
#6682 = DIRECTION ( 'NONE',  ( 0.000000000000000000, 0.000000000000000000, 1.000000000000000000 ) ) ;
#6683 = ORIENTED_EDGE ( 'NONE', *, *, #8598, .F. ) ;
#6684 = DIRECTION ( 'NONE',  ( 0.000000000000000000, -1.000000000000000000, 0.000000000000000000 ) ) ;
#6685 = ORIENTED_EDGE ( 'NONE', *, *, #12535, .F. ) ;
#6686 = CARTESIAN_POINT ( 'NONE',  ( -37.75918829505000218, -6.027090492554000534, 64.85000000000000853 ) ) ;
#6687 = DIRECTION ( 'NONE',  ( 0.000000000000000000, 0.000000000000000000, -1.000000000000000000 ) ) ;
#6688 = CARTESIAN_POINT ( 'NONE',  ( -26.35918829505000005, 10.97290950744599947, 61.86500000000000199 ) ) ;
#6689 = AXIS2_PLACEMENT_3D ( 'NONE', #4233, #6526, #5258 ) ;
#6690 = LINE ( 'NONE', #12072, #2520 ) ;
#6691 = ADVANCED_FACE ( 'NONE', ( #7274 ), #11557, .T. ) ;
#6692 = CARTESIAN_POINT ( 'NONE',  ( -18.05918829504999934, 10.97290950744599947, 60.04999999999999716 ) ) ;
#6693 = ADVANCED_FACE ( 'NONE', ( #3320 ), #10517, .T. ) ;
#6694 = LINE ( 'NONE', #11609, #12730 ) ;
#6695 = DIRECTION ( 'NONE',  ( 0.000000000000000000, 0.000000000000000000, -1.000000000000000000 ) ) ;
#6696 = CARTESIAN_POINT ( 'NONE',  ( 44.63563590245422574, 113.0390816101113387, 0.7500000000000006661 ) ) ;
#6697 = UNCERTAINTY_MEASURE_WITH_UNIT (LENGTH_MEASURE( 1.000000000000000082E-05 ), #9613, 'distance_accuracy_value', 'NONE');
#6698 = VECTOR ( 'NONE', #5695, 1000.000000000000000 ) ;
#6699 = EDGE_CURVE ( 'NONE', #10425, #2443, #13378, .T. ) ;
#6700 = CIRCLE ( 'NONE', #5777, 6.450000000000001066 ) ;
#6701 = AXIS2_PLACEMENT_3D ( 'NONE', #11336, #3041, #4977 ) ;
#6702 = ORIENTED_EDGE ( 'NONE', *, *, #3801, .T. ) ;
#6703 = ORIENTED_EDGE ( 'NONE', *, *, #9094, .T. ) ;
#6704 = DIRECTION ( 'NONE',  ( 0.000000000000000000, 0.000000000000000000, -1.000000000000000000 ) ) ;
#6705 = VERTEX_POINT ( 'NONE', #13653 ) ;
#6706 = VERTEX_POINT ( 'NONE', #948 ) ;
#6707 = FACE_OUTER_BOUND ( 'NONE', #6663, .T. ) ;
#6708 = DIRECTION ( 'NONE',  ( -0.000000000000000000, -0.000000000000000000, 1.000000000000000000 ) ) ;
#6709 = DIRECTION ( 'NONE',  ( 0.000000000000000000, 0.000000000000000000, -1.000000000000000000 ) ) ;
#6710 = ORIENTED_EDGE ( 'NONE', *, *, #9531, .T. ) ;
#6711 = EDGE_CURVE ( 'NONE', #11003, #3675, #4100, .T. ) ;
#6712 = CIRCLE ( 'NONE', #6260, 1.000000000000000000 ) ;
#6713 = VECTOR ( 'NONE', #9560, 1000.000000000000000 ) ;
#6714 = CIRCLE ( 'NONE', #8729, 1.999999999999996669 ) ;
#6715 = FACE_OUTER_BOUND ( 'NONE', #3343, .T. ) ;
#6716 = EDGE_CURVE ( 'NONE', #13212, #5077, #8035, .T. ) ;
#6717 = FACE_OUTER_BOUND ( 'NONE', #12735, .T. ) ;
#6718 = EDGE_CURVE ( 'NONE', #7472, #2002, #13159, .T. ) ;
#6719 = COLOUR_RGB ( '', 0.72549020, 0.75294118, 0.79215686) ;
#6720 = ORIENTED_EDGE ( 'NONE', *, *, #10744, .F. ) ;
#6721 = CARTESIAN_POINT ( 'NONE',  ( -15.85016405347683488, 30.25500104532764212, 60.90324978431328162 ) ) ;
#6722 = VECTOR ( 'NONE', #5392, 1000.000000000000000 ) ;
#6723 = AXIS2_PLACEMENT_3D ( 'NONE', #1205, #9737, #10646 ) ;
#6724 = ORIENTED_EDGE ( 'NONE', *, *, #6569, .F. ) ;
#6725 = ORIENTED_EDGE ( 'NONE', *, *, #5887, .F. ) ;
#6726 = VERTEX_POINT ( 'NONE', #12044 ) ;
#6727 = ORIENTED_EDGE ( 'NONE', *, *, #13461, .F. ) ;
#6728 = CARTESIAN_POINT ( 'NONE',  ( 3.690811704950004657, -6.027090492554000534, 68.85549045786049760 ) ) ;
#6729 = PLANE ( 'NONE',  #8647 ) ;
#6730 = ADVANCED_FACE ( 'NONE', ( #10937 ), #4572, .T. ) ;
#6731 = EDGE_LOOP ( 'NONE', ( #8038, #12339 ) ) ;
#6732 = CARTESIAN_POINT ( 'NONE',  ( -11.46335496205000126, 10.97290950744599947, 60.40999999999999659 ) ) ;
#6733 = CARTESIAN_POINT ( 'NONE',  ( -16.64497473267689998, 26.91028695795525039, 56.84999999999999432 ) ) ;
#6734 = CARTESIAN_POINT ( 'NONE',  ( -18.05918829504999934, 10.97290950744599947, 68.84999999999999432 ) ) ;
#6735 = FACE_OUTER_BOUND ( 'NONE', #2895, .T. ) ;
#6736 = ADVANCED_FACE ( 'NONE', ( #12116 ), #3394, .T. ) ;
#6737 = ORIENTED_EDGE ( 'NONE', *, *, #10076, .T. ) ;
#6738 = ORIENTED_EDGE ( 'NONE', *, *, #5831, .F. ) ;
#6739 = ORIENTED_EDGE ( 'NONE', *, *, #9102, .F. ) ;
#6740 = CONICAL_SURFACE ( 'NONE', #5615, 7.618085573000000110, 0.1329427246665018103 ) ;
#6741 = CARTESIAN_POINT ( 'NONE',  ( 1.097360187335109982, -3.327306731351814761, 7.250000000000000000 ) ) ;
#6742 = ORIENTED_EDGE ( 'NONE', *, *, #10839, .F. ) ;
#6743 = CARTESIAN_POINT ( 'NONE',  ( 68.49370948373500312, 75.03908161011133870, 0.000000000000000000 ) ) ;
#6744 = EDGE_CURVE ( 'NONE', #3046, #3872, #12284, .T. ) ;
#6745 = CARTESIAN_POINT ( 'NONE',  ( -21.37114540074985314, 30.12306837294896056, 55.16656713510205634 ) ) ;
#6746 = CARTESIAN_POINT ( 'NONE',  ( 68.49370948373500312, 85.78908161011133870, 0.7500000000000000000 ) ) ;
#6747 = VERTEX_POINT ( 'NONE', #11009 ) ;
#6748 = DIRECTION ( 'NONE',  ( 0.000000000000000000, 0.000000000000000000, 1.000000000000000000 ) ) ;
#6749 = DIRECTION ( 'NONE',  ( 1.000000000000000000, 0.000000000000000000, 0.000000000000000000 ) ) ;
#6750 = DIRECTION ( 'NONE',  ( 0.000000000000000000, 0.000000000000000000, 1.000000000000000000 ) ) ;
#6751 = DIRECTION ( 'NONE',  ( 1.224646799147353207E-16, 1.000000000000000000, -0.000000000000000000 ) ) ;
#6752 = EDGE_CURVE ( 'NONE', #4217, #6, #12181, .T. ) ;
#6753 = VECTOR ( 'NONE', #1706, 1000.000000000000000 ) ;
#6754 = ORIENTED_EDGE ( 'NONE', *, *, #7199, .T. ) ;
#6755 = DIRECTION ( 'NONE',  ( 0.000000000000000000, 0.000000000000000000, 1.000000000000000000 ) ) ;
#6756 = DIRECTION ( 'NONE',  ( 0.000000000000000000, 0.000000000000000000, -1.000000000000000000 ) ) ;
#6757 = ORIENTED_EDGE ( 'NONE', *, *, #4180, .T. ) ;
#6758 = DIRECTION ( 'NONE',  ( -0.000000000000000000, 1.000000000000000000, -0.000000000000000000 ) ) ;
#6759 = CARTESIAN_POINT ( 'NONE',  ( -16.08092853089235774, 4.500000000000000000, 9.237812082545083570 ) ) ;
#6760 = DIRECTION ( 'NONE',  ( 0.000000000000000000, 0.000000000000000000, -1.000000000000000000 ) ) ;
#6761 = CIRCLE ( 'NONE', #7404, 23.49999999999999645 ) ;
#6762 = PLANE ( 'NONE',  #3165 ) ;
#6763 = CARTESIAN_POINT ( 'NONE',  ( -35.05918829505000645, 27.97290950744599769, 58.85000000000000142 ) ) ;
#6764 = CARTESIAN_POINT ( 'NONE',  ( 140.6356359024541973, 103.9054980190242361, 22.75000000000000000 ) ) ;
#6765 = DIRECTION ( 'NONE',  ( 0.000000000000000000, 0.000000000000000000, -1.000000000000000000 ) ) ;
#6766 = PLANE ( 'NONE',  #9851 ) ;
#6767 = DIRECTION ( 'NONE',  ( 0.000000000000000000, 0.000000000000000000, -1.000000000000000000 ) ) ;
#6768 = DIRECTION ( 'NONE',  ( 0.000000000000000000, 0.000000000000000000, 1.000000000000000000 ) ) ;
#6769 = AXIS2_PLACEMENT_3D ( 'NONE', #8935, #13192, #3642 ) ;
#6770 = EDGE_CURVE ( 'NONE', #973, #51, #1352, .T. ) ;
#6771 = FACE_OUTER_BOUND ( 'NONE', #512, .T. ) ;
#6772 = ORIENTED_EDGE ( 'NONE', *, *, #9101, .F. ) ;
#6773 = ORIENTED_EDGE ( 'NONE', *, *, #12076, .F. ) ;
#6774 = LINE ( 'NONE', #3776, #7945 ) ;
#6775 = DIRECTION ( 'NONE',  ( 0.000000000000000000, 0.000000000000000000, -1.000000000000000000 ) ) ;
#6776 = CARTESIAN_POINT ( 'NONE',  ( 140.3856359024541973, 104.1554980190242361, 23.00000000000000000 ) ) ;
#6777 = FACE_OUTER_BOUND ( 'NONE', #13645, .T. ) ;
#6778 = PLANE ( 'NONE',  #2704 ) ;
#6779 = FACE_BOUND ( 'NONE', #13161, .T. ) ;
#6780 = VECTOR ( 'NONE', #250, 1000.000000000000000 ) ;
#6781 = ADVANCED_FACE ( 'NONE', ( #6735 ), #11972, .F. ) ;
#6782 = CARTESIAN_POINT ( 'NONE',  ( -14.32322260522609980, 18.32852371459815188, 60.04999999999999716 ) ) ;
#6783 = VERTEX_POINT ( 'NONE', #1424 ) ;
#6784 = VERTEX_POINT ( 'NONE', #9950 ) ;
#6785 = ORIENTED_EDGE ( 'NONE', *, *, #11763, .T. ) ;
#6786 = ORIENTED_EDGE ( 'NONE', *, *, #9499, .T. ) ;
#6787 = ORIENTED_EDGE ( 'NONE', *, *, #1883, .T. ) ;
#6788 = PLANE ( 'NONE',  #1298 ) ;
#6789 = DIRECTION ( 'NONE',  ( 0.000000000000000000, 0.000000000000000000, 1.000000000000000000 ) ) ;
#6790 = ORIENTED_EDGE ( 'NONE', *, *, #3636, .F. ) ;
#6791 = CARTESIAN_POINT ( 'NONE',  ( -18.05918829504999934, 10.97290950744599947, 116.8499999999999943 ) ) ;
#6792 = DIRECTION ( 'NONE',  ( -0.000000000000000000, -0.000000000000000000, -1.000000000000000000 ) ) ;
#6793 = FACE_OUTER_BOUND ( 'NONE', #13235, .T. ) ;
#6794 = CARTESIAN_POINT ( 'NONE',  ( -16.07440008066354764, 8.723328269963658954, 27.09999999999999787 ) ) ;
#6795 = CIRCLE ( 'NONE', #11049, 3.000000000000000888 ) ;
#6796 = ORIENTED_EDGE ( 'NONE', *, *, #7448, .T. ) ;
#6797 = ADVANCED_FACE ( 'NONE', ( #2634 ), #11069, .F. ) ;
#6798 = ORIENTED_EDGE ( 'NONE', *, *, #4180, .F. ) ;
#6799 = ADVANCED_FACE ( 'NONE', ( #375 ), #10712, .T. ) ;
#6800 = DIRECTION ( 'NONE',  ( -1.000000000000000000, 0.000000000000000000, 0.000000000000000000 ) ) ;
#6801 = ORIENTED_EDGE ( 'NONE', *, *, #6699, .T. ) ;
#6802 = EDGE_CURVE ( 'NONE', #5819, #9940, #7688, .T. ) ;
#6803 = AXIS2_PLACEMENT_3D ( 'NONE', #3500, #11043, #2470 ) ;
#6804 = CARTESIAN_POINT ( 'NONE',  ( -21.64539278097895902, 30.08178984978753689, 58.87173069243009138 ) ) ;
#6805 = DIRECTION ( 'NONE',  ( 0.000000000000000000, 0.000000000000000000, 1.000000000000000000 ) ) ;
#6806 = DIRECTION ( 'NONE',  ( -0.7071067811865525687, -0.7071067811865425767, 0.000000000000000000 ) ) ;
#6807 = DIRECTION ( 'NONE',  ( 0.000000000000000000, 0.000000000000000000, -1.000000000000000000 ) ) ;
#6808 = DIRECTION ( 'NONE',  ( 0.000000000000000000, 0.000000000000000000, 1.000000000000000000 ) ) ;
#6809 = DIRECTION ( 'NONE',  ( 0.000000000000000000, 0.000000000000000000, -1.000000000000000000 ) ) ;
#6810 = ORIENTED_EDGE ( 'NONE', *, *, #7743, .T. ) ;
#6811 = ORIENTED_EDGE ( 'NONE', *, *, #414, .T. ) ;
#6812 = EDGE_CURVE ( 'NONE', #5535, #6329, #12046, .T. ) ;
#6813 = AXIS2_PLACEMENT_3D ( 'NONE', #4868, #7016, #6953 ) ;
#6814 = EDGE_LOOP ( 'NONE', ( #10011, #7646, #7856, #5419 ) ) ;
#6815 = CARTESIAN_POINT ( 'NONE',  ( 8.500000000000003553, 2.500000000000000000, -65.00000000000000000 ) ) ;
#6816 = DIRECTION ( 'NONE',  ( 0.000000000000000000, 0.000000000000000000, 1.000000000000000000 ) ) ;
#6817 = VERTEX_POINT ( 'NONE', #448 ) ;
#6818 = DIRECTION ( 'NONE',  ( -0.3202092937642119774, -0.6304490528084099044, 0.7071067811865499042 ) ) ;
#6819 = DIRECTION ( 'NONE',  ( 0.000000000000000000, 0.000000000000000000, 1.000000000000000000 ) ) ;
#6820 = EDGE_CURVE ( 'NONE', #10750, #4939, #4434, .T. ) ;
#6821 = CARTESIAN_POINT ( 'NONE',  ( 109.1537879975201406, 115.4601262030644762, 0.000000000000000000 ) ) ;
#6822 = DIRECTION ( 'NONE',  ( 0.000000000000000000, 0.000000000000000000, 1.000000000000000000 ) ) ;
#6823 = DIRECTION ( 'NONE',  ( -0.000000000000000000, -0.000000000000000000, -1.000000000000000000 ) ) ;
#6824 = LINE ( 'NONE', #6764, #1993 ) ;
#6825 = CARTESIAN_POINT ( 'NONE',  ( 68.49370948373500312, 123.0390816101113245, 0.7500000000000006661 ) ) ;
#6826 = DIRECTION ( 'NONE',  ( -0.9496839325805410681, 0.3132098788326420635, 0.000000000000000000 ) ) ;
#6827 = CARTESIAN_POINT ( 'NONE',  ( 42.63563590245419732, 87.03908161011138134, 0.3106601717798216367 ) ) ;
#6828 = CARTESIAN_POINT ( 'NONE',  ( -18.05918829504999934, 10.97290950744599947, 60.04999999999999716 ) ) ;
#6829 = VERTEX_POINT ( 'NONE', #5608 ) ;
#6830 = AXIS2_PLACEMENT_3D ( 'NONE', #2607, #9927, #3852 ) ;
#6831 = ORIENTED_EDGE ( 'NONE', *, *, #8957, .F. ) ;
#6832 = ORIENTED_EDGE ( 'NONE', *, *, #904, .T. ) ;
#6833 = DIRECTION ( 'NONE',  ( 0.000000000000000000, 0.000000000000000000, 1.000000000000000000 ) ) ;
#6834 = ORIENTED_EDGE ( 'NONE', *, *, #5096, .F. ) ;
#6835 = CARTESIAN_POINT ( 'NONE',  ( -18.05918829504999934, 10.97290950744599947, 0.000000000000000000 ) ) ;
#6836 = ADVANCED_FACE ( 'NONE', ( #8973 ), #7131, .F. ) ;
#6837 = LINE ( 'NONE', #5993, #4708 ) ;
#6838 = SURFACE_STYLE_FILL_AREA ( #4819 ) ;
#6839 = DIRECTION ( 'NONE',  ( 1.000000000000000000, 0.000000000000000000, 0.000000000000000000 ) ) ;
#6840 = FACE_OUTER_BOUND ( 'NONE', #5411, .T. ) ;
#6841 = AXIS2_PLACEMENT_3D ( 'NONE', #9206, #3070, #11573 ) ;
#6842 = DIRECTION ( 'NONE',  ( 0.000000000000000000, 1.000000000000000000, 0.000000000000000000 ) ) ;
#6843 = EDGE_LOOP ( 'NONE', ( #13346, #13405, #4767, #1105 ) ) ;
#6844 = ORIENTED_EDGE ( 'NONE', *, *, #11587, .F. ) ;
#6845 = ORIENTED_EDGE ( 'NONE', *, *, #4763, .T. ) ;
#6846 = CARTESIAN_POINT ( 'NONE',  ( -16.51503883096479441, 30.30889438433393224, 61.33492039510051086 ) ) ;
#6847 = ORIENTED_EDGE ( 'NONE', *, *, #4162, .F. ) ;
#6848 = VERTEX_POINT ( 'NONE', #6860 ) ;
#6849 = EDGE_LOOP ( 'NONE', ( #6967, #441 ) ) ;
#6850 = VERTEX_POINT ( 'NONE', #6656 ) ;
#6851 = ORIENTED_EDGE ( 'NONE', *, *, #6435, .T. ) ;
#6852 = DIRECTION ( 'NONE',  ( 0.000000000000000000, 0.000000000000000000, -1.000000000000000000 ) ) ;
#6853 = LINE ( 'NONE', #8891, #12677 ) ;
#6854 = ORIENTED_EDGE ( 'NONE', *, *, #7984, .F. ) ;
#6855 = DIRECTION ( 'NONE',  ( -1.000000000000000000, 0.000000000000000000, 0.000000000000000000 ) ) ;
#6856 = CARTESIAN_POINT ( 'NONE',  ( -1.059188295049996231, -6.027090492554000534, 58.85000000000000142 ) ) ;
#6857 = EDGE_CURVE ( 'NONE', #10151, #12033, #11137, .T. ) ;
#6858 = DIRECTION ( 'NONE',  ( -0.4528443260392609471, -0.8915896008669278450, 0.000000000000000000 ) ) ;
#6859 = ADVANCED_FACE ( 'NONE', ( #156 ), #12945, .T. ) ;
#6860 = CARTESIAN_POINT ( 'NONE',  ( -16.08092853089235774, 0.000000000000000000, 11.23781208254507469 ) ) ;
#6861 = CIRCLE ( 'NONE', #5292, 10.74999999999999645 ) ;
#6862 = AXIS2_PLACEMENT_3D ( 'NONE', #10852, #11826, #8604 ) ;
#6863 = VECTOR ( 'NONE', #2505, 1000.000000000000114 ) ;
#6864 = ORIENTED_EDGE ( 'NONE', *, *, #2556, .T. ) ;
#6865 = ORIENTED_EDGE ( 'NONE', *, *, #6744, .T. ) ;
#6866 = LINE ( 'NONE', #7774, #11075 ) ;
#6867 = VECTOR ( 'NONE', #5529, 1000.000000000000000 ) ;
#6868 = AXIS2_PLACEMENT_3D ( 'NONE', #3933, #13627, #13694 ) ;
#6869 = EDGE_LOOP ( 'NONE', ( #1011, #1996 ) ) ;
#6870 = CIRCLE ( 'NONE', #7988, 23.29163056034261459 ) ;
#6871 = DIRECTION ( 'NONE',  ( 0.000000000000000000, 0.000000000000000000, 1.000000000000000000 ) ) ;
#6872 = VECTOR ( 'NONE', #4226, 1000.000000000000000 ) ;
#6873 = CARTESIAN_POINT ( 'NONE',  ( -21.32667269782450603, 30.12932847811543269, 59.61340462581008381 ) ) ;
#6874 = CARTESIAN_POINT ( 'NONE',  ( 134.6356359024541973, 89.90549801902423610, 20.00000000000000000 ) ) ;
#6875 = DIRECTION ( 'NONE',  ( 0.000000000000000000, 0.000000000000000000, 1.000000000000000000 ) ) ;
#6876 = FACE_OUTER_BOUND ( 'NONE', #2292, .T. ) ;
#6877 = EDGE_CURVE ( 'NONE', #2075, #9462, #5348, .T. ) ;
#6878 = DIRECTION ( 'NONE',  ( -1.000000000000000000, 0.000000000000000000, 0.000000000000000000 ) ) ;
#6879 = CARTESIAN_POINT ( 'NONE',  ( -110.6948241975042322, -88.06617210266534812, 78.85000000000000853 ) ) ;
#6880 = VECTOR ( 'NONE', #10476, 1000.000000000000000 ) ;
#6881 = VECTOR ( 'NONE', #13241, 1000.000000000000000 ) ;
#6882 = AXIS2_PLACEMENT_3D ( 'NONE', #7447, #13628, #5240 ) ;
#6883 = ADVANCED_FACE ( 'NONE', ( #4917 ), #7198, .F. ) ;
#6884 = VERTEX_POINT ( 'NONE', #11410 ) ;
#6885 = DIRECTION ( 'NONE',  ( 0.000000000000000000, 0.000000000000000000, 1.000000000000000000 ) ) ;
#6886 = APPLICATION_CONTEXT ( 'automotive_design' ) ;
#6887 = CARTESIAN_POINT ( 'NONE',  ( 74.18094369249178044, 97.20665973629650125, 10.00000000000000000 ) ) ;
#6888 = LINE ( 'NONE', #13311, #7572 ) ;
#6889 = DIRECTION ( 'NONE',  ( 0.000000000000000000, 1.000000000000000000, 0.000000000000000000 ) ) ;
#6890 = LINE ( 'NONE', #11156, #623 ) ;
#6891 = PLANE ( 'NONE',  #7575 ) ;
#6892 = CARTESIAN_POINT ( 'NONE',  ( -18.05918829504999934, 10.97290950744599947, 23.90000000000000213 ) ) ;
#6893 = DIRECTION ( 'NONE',  ( 0.000000000000000000, 0.000000000000000000, 1.000000000000000000 ) ) ;
#6894 = DIRECTION ( 'NONE',  ( 0.4528443260392610026, 0.8915896008669278450, 0.000000000000000000 ) ) ;
#6895 = CARTESIAN_POINT ( 'NONE',  ( -35.05918829505000645, -6.027090492554000534, 7.250000000000000000 ) ) ;
#6896 = EDGE_CURVE ( 'NONE', #4292, #859, #11159, .T. ) ;
#6897 = CARTESIAN_POINT ( 'NONE',  ( -18.05918829504999934, 10.97290950744599947, 60.40999999999999659 ) ) ;
#6898 = AXIS2_PLACEMENT_3D ( 'NONE', #11272, #1844, #4916 ) ;
#6899 = DIRECTION ( 'NONE',  ( 0.000000000000000000, -1.000000000000000000, 0.000000000000000000 ) ) ;
#6900 = EDGE_CURVE ( 'NONE', #719, #182, #4012, .T. ) ;
#6901 = ORIENTED_EDGE ( 'NONE', *, *, #7381, .F. ) ;
#6902 = ORIENTED_EDGE ( 'NONE', *, *, #7436, .F. ) ;
#6903 = AXIS2_PLACEMENT_3D ( 'NONE', #11614, #6568, #1254 ) ;
#6904 = FACE_OUTER_BOUND ( 'NONE', #8782, .T. ) ;
#6905 = CIRCLE ( 'NONE', #8689, 33.00000000000000000 ) ;
#6906 = DIRECTION ( 'NONE',  ( 0.000000000000000000, 0.000000000000000000, -1.000000000000000000 ) ) ;
#6907 = CARTESIAN_POINT ( 'NONE',  ( 140.3249757306743675, 85.78908161011133870, 0.000000000000000000 ) ) ;
#6908 = CARTESIAN_POINT ( 'NONE',  ( -37.75918829505000218, 27.97290950744599769, 7.250000000000000000 ) ) ;
#6909 = EDGE_CURVE ( 'NONE', #6747, #1393, #12297, .T. ) ;
#6910 = CARTESIAN_POINT ( 'NONE',  ( -18.05918829504999934, 2.892876190446000084, 63.34900083300000517 ) ) ;
#6911 = DIRECTION ( 'NONE',  ( 0.4528443260392608360, 0.8915896008669278450, 0.000000000000000000 ) ) ;
#6912 = DIRECTION ( 'NONE',  ( -1.000000000000000000, 0.000000000000000000, 0.000000000000000000 ) ) ;
#6913 = AXIS2_PLACEMENT_3D ( 'NONE', #13517, #3960, #4799 ) ;
#6914 = AXIS2_PLACEMENT_3D ( 'NONE', #9013, #4895, #11253 ) ;
#6915 = AXIS2_PLACEMENT_3D ( 'NONE', #2984, #11273, #785 ) ;
#6916 = EDGE_CURVE ( 'NONE', #11045, #952, #6700, .T. ) ;
#6917 = ORIENTED_EDGE ( 'NONE', *, *, #8087, .T. ) ;
#6918 = CARTESIAN_POINT ( 'NONE',  ( -17.27672718608728886, 30.34709526170184546, 61.61607410999997114 ) ) ;
#6919 = VERTEX_POINT ( 'NONE', #11476 ) ;
#6920 = ORIENTED_EDGE ( 'NONE', *, *, #5498, .F. ) ;
#6921 = ORIENTED_EDGE ( 'NONE', *, *, #4989, .T. ) ;
#6922 = VECTOR ( 'NONE', #8620, 1000.000000000000000 ) ;
#6923 = CYLINDRICAL_SURFACE ( 'NONE', #2621, 0.7500000000000006661 ) ;
#6924 = ORIENTED_EDGE ( 'NONE', *, *, #12631, .F. ) ;
#6925 = AXIS2_PLACEMENT_3D ( 'NONE', #5115, #8333, #5379 ) ;
#6926 = CARTESIAN_POINT ( 'NONE',  ( -34.72201093190195564, 10.97290950744599947, 17.25000000000000000 ) ) ;
#6927 = AXIS2_PLACEMENT_3D ( 'NONE', #9380, #4083, #8329 ) ;
#6928 = DIRECTION ( 'NONE',  ( 1.000000000000000000, 0.000000000000000000, -0.000000000000000000 ) ) ;
#6929 = CARTESIAN_POINT ( 'NONE',  ( -25.86749127492454647, -8.860076549334127805, 83.57661607529820458 ) ) ;
#6930 = CARTESIAN_POINT ( 'NONE',  ( 79.82136590429890077, 114.1051029460540605, 10.00000000000000000 ) ) ;
#6931 = CARTESIAN_POINT ( 'NONE',  ( -18.05918829504999934, 10.97290950744599947, 61.86500000000000199 ) ) ;
#6932 = CARTESIAN_POINT ( 'NONE',  ( -5.640422211807260666, -16.89844320975769776, 7.000000000000000000 ) ) ;
#6933 = CYLINDRICAL_SURFACE ( 'NONE', #2940, 0.7499999999999973355 ) ;
#6934 = VECTOR ( 'NONE', #11498, 1000.000000000000000 ) ;
#6935 = AXIS2_PLACEMENT_3D ( 'NONE', #5253, #4365, #10643 ) ;
#6936 = VECTOR ( 'NONE', #2160, 1000.000000000000000 ) ;
#6937 = ORIENTED_EDGE ( 'NONE', *, *, #972, .T. ) ;
#6938 = ORIENTED_EDGE ( 'NONE', *, *, #400, .F. ) ;
#6939 = EDGE_CURVE ( 'NONE', #1440, #8302, #9163, .T. ) ;
#6940 = DIRECTION ( 'NONE',  ( -1.000000000000000000, 0.000000000000000000, 0.000000000000000000 ) ) ;
#6941 = EDGE_LOOP ( 'NONE', ( #5424, #7190 ) ) ;
#6942 =( LENGTH_UNIT ( ) NAMED_UNIT ( * ) SI_UNIT ( .MILLI., .METRE. ) );
#6943 = CARTESIAN_POINT ( 'NONE',  ( -20.86626825454071010, 30.19004818229314324, 60.30515349700372951 ) ) ;
#6944 = CIRCLE ( 'NONE', #8727, 9.999999999999994671 ) ;
#6945 =( BOUNDED_CURVE ( )  B_SPLINE_CURVE ( 3, ( #6973, #13203, #620, #11251 ),
 .UNSPECIFIED., .F., .F. ) 
 B_SPLINE_CURVE_WITH_KNOTS ( ( 4, 4 ),
 ( 3.141592653589793116, 4.712388980384689674 ),
 .UNSPECIFIED. ) 
 CURVE ( )  GEOMETRIC_REPRESENTATION_ITEM ( )  RATIONAL_B_SPLINE_CURVE ( ( 1.000000000000000000, 0.8047378541243649375, 0.8047378541243649375, 1.000000000000000000 ) ) 
 REPRESENTATION_ITEM ( '' )  );
#6946 = VECTOR ( 'NONE', #13012, 1000.000000000000000 ) ;
#6947 = FACE_OUTER_BOUND ( 'NONE', #6607, .T. ) ;
#6948 = CARTESIAN_POINT ( 'NONE',  ( -5.631644894983189431, 10.97290950744599947, 17.25000000000000000 ) ) ;
#6949 = CARTESIAN_POINT ( 'NONE',  ( -35.05918829505000645, 27.97290950744599769, 7.250000000000000000 ) ) ;
#6950 = CYLINDRICAL_SURFACE ( 'NONE', #10269, 0.5000000000000004441 ) ;
#6951 = VECTOR ( 'NONE', #4803, 1000.000000000000000 ) ;
#6952 = ADVANCED_FACE ( 'NONE', ( #7000 ), #6933, .T. ) ;
#6953 = DIRECTION ( 'NONE',  ( 1.000000000000000000, 0.000000000000000000, 0.000000000000000000 ) ) ;
#6954 = PLANE ( 'NONE',  #5351 ) ;
#6955 = ORIENTED_EDGE ( 'NONE', *, *, #5607, .F. ) ;
#6956 = CARTESIAN_POINT ( 'NONE',  ( 50.63563590245420443, 94.90549801902425031, 20.00000000000000000 ) ) ;
#6957 = SURFACE_STYLE_USAGE ( .BOTH. , #3756 ) ;
#6958 = DIRECTION ( 'NONE',  ( -0.000000000000000000, -0.000000000000000000, 1.000000000000000000 ) ) ;
#6959 = CARTESIAN_POINT ( 'NONE',  ( 5.999999999999999112, -12.00000000000000178, 7.000000000000000000 ) ) ;
#6960 = CARTESIAN_POINT ( 'NONE',  ( 42.94629607423402007, 110.9104019536709842, 20.00000000000000000 ) ) ;
#6961 = DIRECTION ( 'NONE',  ( -1.000000000000000000, 0.000000000000000000, 0.000000000000000000 ) ) ;
#6962 = DIRECTION ( 'NONE',  ( 0.000000000000000000, 0.000000000000000000, 1.000000000000000000 ) ) ;
#6963 = LINE ( 'NONE', #11303, #11839 ) ;
#6964 = VECTOR ( 'NONE', #7702, 1000.000000000000000 ) ;
#6965 = DIRECTION ( 'NONE',  ( 0.000000000000000000, 0.000000000000000000, -1.000000000000000000 ) ) ;
#6966 = CARTESIAN_POINT ( 'NONE',  ( 141.8856359024541973, 87.34974178189115435, 0.000000000000000000 ) ) ;
#6967 = ORIENTED_EDGE ( 'NONE', *, *, #1598, .T. ) ;
#6968 = ADVANCED_FACE ( 'NONE', ( #12529 ), #8127, .F. ) ;
#6969 = CYLINDRICAL_SURFACE ( 'NONE', #12168, 33.00000000000000000 ) ;
#6970 = ORIENTED_EDGE ( 'NONE', *, *, #10164, .T. ) ;
#6971 = VERTEX_POINT ( 'NONE', #583 ) ;
#6972 = ORIENTED_EDGE ( 'NONE', *, *, #4225, .F. ) ;
#6973 = CARTESIAN_POINT ( 'NONE',  ( 134.6356359024541973, 103.9054980190242361, 22.75000000000000000 ) ) ;
#6974 = CARTESIAN_POINT ( 'NONE',  ( -38.05918829505000645, 27.97290950744599769, 0.000000000000000000 ) ) ;
#6975 = DIRECTION ( 'NONE',  ( -1.000000000000000000, 0.000000000000000000, 0.000000000000000000 ) ) ;
#6976 = CARTESIAN_POINT ( 'NONE',  ( 113.0903281124166710, 100.8715034839261762, 10.00000000000000000 ) ) ;
#6977 = EDGE_CURVE ( 'NONE', #5932, #8025, #1778, .T. ) ;
#6978 = CARTESIAN_POINT ( 'NONE',  ( -30.48673169511680214, 10.97290950744599947, 64.85000000000000853 ) ) ;
#6979 = DIRECTION ( 'NONE',  ( 0.000000000000000000, 0.000000000000000000, -1.000000000000000000 ) ) ;
#6980 = CARTESIAN_POINT ( 'NONE',  ( 76.11748380738829667, 82.61803701715820125, 20.00000000000000000 ) ) ;
#6981 = ORIENTED_EDGE ( 'NONE', *, *, #2180, .F. ) ;
#6982 = ORIENTED_EDGE ( 'NONE', *, *, #5555, .F. ) ;
#6983 = EDGE_CURVE ( 'NONE', #3980, #13266, #7064, .T. ) ;
#6984 = ORIENTED_EDGE ( 'NONE', *, *, #636, .T. ) ;
#6985 = CARTESIAN_POINT ( 'NONE',  ( -1.059188295049996231, 27.97290950744599769, 64.85000000000000853 ) ) ;
#6986 = VERTEX_POINT ( 'NONE', #4981 ) ;
#6987 = ORIENTED_EDGE ( 'NONE', *, *, #10254, .T. ) ;
#6988 =( NAMED_UNIT ( * ) PLANE_ANGLE_UNIT ( ) SI_UNIT ( $, .RADIAN. ) );
#6989 = ORIENTED_EDGE ( 'NONE', *, *, #5832, .T. ) ;
#6990 = CYLINDRICAL_SURFACE ( 'NONE', #9848, 5.000000000000000888 ) ;
#6991 = ORIENTED_EDGE ( 'NONE', *, *, #6569, .T. ) ;
#6992 = CIRCLE ( 'NONE', #981, 4.750000000000000888 ) ;
#6993 = CARTESIAN_POINT ( 'NONE',  ( -24.10918829505000005, 10.97290950744599947, 0.000000000000000000 ) ) ;
#6994 = CARTESIAN_POINT ( 'NONE',  ( 142.3249757306743675, 87.16776126655166479, 2.983588460272618114E-16 ) ) ;
#6995 = EDGE_CURVE ( 'NONE', #12924, #8537, #9606, .T. ) ;
#6996 = CARTESIAN_POINT ( 'NONE',  ( -17.23821357112329977, 5.029341513162310484, 64.85000000000000853 ) ) ;
#6997 = CARTESIAN_POINT ( 'NONE',  ( -18.05918829504999934, 30.36027202460864771, 61.70913974837019822 ) ) ;
#6998 = EDGE_CURVE ( 'NONE', #11514, #2014, #3940, .T. ) ;
#6999 = CARTESIAN_POINT ( 'NONE',  ( -17.14002684535937604, 27.94862847170599096, 58.55192794567741288 ) ) ;
#7000 = FACE_OUTER_BOUND ( 'NONE', #12972, .T. ) ;
#7001 = ORIENTED_EDGE ( 'NONE', *, *, #11759, .F. ) ;
#7002 = ORIENTED_EDGE ( 'NONE', *, *, #497, .T. ) ;
#7003 = ORIENTED_EDGE ( 'NONE', *, *, #2930, .F. ) ;
#7004 = ORIENTED_EDGE ( 'NONE', *, *, #3910, .F. ) ;
#7005 = DIRECTION ( 'NONE',  ( 0.000000000000000000, 0.000000000000000000, 1.000000000000000000 ) ) ;
#7006 = CARTESIAN_POINT ( 'NONE',  ( -18.05918829504999934, 10.97290950744599947, 7.250000000000000000 ) ) ;
#7007 = DIRECTION ( 'NONE',  ( 0.000000000000000000, 1.000000000000000000, 0.000000000000000000 ) ) ;
#7008 = DIRECTION ( 'NONE',  ( 1.000000000000000000, 3.614007241618347908E-17, 0.000000000000000000 ) ) ;
#7009 = CARTESIAN_POINT ( 'NONE',  ( -12.00000000000000000, -2.500000000000000444, -65.00000000000000000 ) ) ;
#7010 = DIRECTION ( 'NONE',  ( 1.000000000000000000, 0.000000000000000000, 0.000000000000000000 ) ) ;
#7011 = ORIENTED_EDGE ( 'NONE', *, *, #4569, .F. ) ;
#7012 = EDGE_CURVE ( 'NONE', #2384, #12649, #3152, .T. ) ;
#7013 = ORIENTED_EDGE ( 'NONE', *, *, #4413, .F. ) ;
#7014 = CLOSED_SHELL ( 'NONE', ( #1795, #1093, #4105, #9200, #2378, #9800 ) ) ;
#7015 = AXIS2_PLACEMENT_3D ( 'NONE', #10145, #6440, #1338 ) ;
#7016 = DIRECTION ( 'NONE',  ( 0.000000000000000000, 0.000000000000000000, 1.000000000000000000 ) ) ;
#7017 = ORIENTED_EDGE ( 'NONE', *, *, #2311, .F. ) ;
#7018 = ORIENTED_EDGE ( 'NONE', *, *, #11053, .T. ) ;
#7019 = FACE_OUTER_BOUND ( 'NONE', #10366, .T. ) ;
#7020 = DIRECTION ( 'NONE',  ( -1.000000000000000000, 0.000000000000000000, 0.000000000000000000 ) ) ;
#7021 = PLANE ( 'NONE',  #12008 ) ;
#7022 = FACE_OUTER_BOUND ( 'NONE', #3047, .T. ) ;
#7023 = CARTESIAN_POINT ( 'NONE',  ( 43.38563590245419732, 110.7284214383315089, 20.00000000000000000 ) ) ;
#7024 = DIRECTION ( 'NONE',  ( 0.000000000000000000, 0.000000000000000000, -1.000000000000000000 ) ) ;
#7025 = DIRECTION ( 'NONE',  ( 1.000000000000000000, -0.000000000000000000, 0.000000000000000000 ) ) ;
#7026 = DIRECTION ( 'NONE',  ( 1.000000000000000000, 0.000000000000000000, 0.000000000000000000 ) ) ;
#7027 = CARTESIAN_POINT ( 'NONE',  ( 92.63563590245421153, 99.03908161011133870, 20.00000000000000000 ) ) ;
#7028 = EDGE_CURVE ( 'NONE', #7612, #9617, #12254, .T. ) ;
#7029 = EDGE_CURVE ( 'NONE', #11722, #6318, #907, .T. ) ;
#7030 = CIRCLE ( 'NONE', #6368, 16.95000000000000284 ) ;
#7031 = EDGE_CURVE ( 'NONE', #4495, #9970, #8095, .T. ) ;
#7032 = EDGE_LOOP ( 'NONE', ( #10004, #11262, #9503, #11571 ) ) ;
#7033 = ORIENTED_EDGE ( 'NONE', *, *, #4782, .F. ) ;
#7034 = ORIENTED_EDGE ( 'NONE', *, *, #9594, .F. ) ;
#7035 = FACE_OUTER_BOUND ( 'NONE', #6214, .T. ) ;
#7036 = ORIENTED_EDGE ( 'NONE', *, *, #3860, .F. ) ;
#7037 = DIRECTION ( 'NONE',  ( 1.000000000000000000, 0.000000000000000000, 0.000000000000000000 ) ) ;
#7038 = AXIS2_PLACEMENT_3D ( 'NONE', #4311, #7554, #5333 ) ;
#7039 = CARTESIAN_POINT ( 'NONE',  ( -8.814269998155332075, 15.06602133594271820, -3.000000000000000000 ) ) ;
#7040 = DIRECTION ( 'NONE',  ( -0.6615960714621564875, 0.7498604124941129490, 0.000000000000000000 ) ) ;
#7041 = CARTESIAN_POINT ( 'NONE',  ( 134.6356359024541973, 108.9054980190242503, 22.75000000000000000 ) ) ;
#7042 = DIRECTION ( 'NONE',  ( -1.000000000000000000, 0.000000000000000000, 0.000000000000000000 ) ) ;
#7043 = DIRECTION ( 'NONE',  ( 1.000000000000000000, 0.000000000000000000, 0.000000000000000000 ) ) ;
#7044 = ADVANCED_FACE ( 'NONE', ( #5813, #10231 ), #6433, .F. ) ;
#7045 = CARTESIAN_POINT ( 'NONE',  ( 42.63563590245419732, 85.03908161011133870, 20.00000000000000000 ) ) ;
#7046 = AXIS2_PLACEMENT_3D ( 'NONE', #13622, #8250, #12722 ) ;
#7047 = ADVANCED_FACE ( 'NONE', ( #8397 ), #4086, .T. ) ;
#7048 = ORIENTED_EDGE ( 'NONE', *, *, #11486, .F. ) ;
#7049 = ORIENTED_EDGE ( 'NONE', *, *, #5729, .F. ) ;
#7050 = CARTESIAN_POINT ( 'NONE',  ( -14.22822014949529112, 30.04220389463379703, 57.85890972080246542 ) ) ;
#7051 = VERTEX_POINT ( 'NONE', #9387 ) ;
#7052 = DIRECTION ( 'NONE',  ( 0.000000000000000000, 0.000000000000000000, -1.000000000000000000 ) ) ;
#7053 = DIRECTION ( 'NONE',  ( 0.000000000000000000, 0.000000000000000000, -1.000000000000000000 ) ) ;
#7054 = ORIENTED_EDGE ( 'NONE', *, *, #3973, .F. ) ;
#7055 = ORIENTED_EDGE ( 'NONE', *, *, #11747, .F. ) ;
#7056 = FACE_OUTER_BOUND ( 'NONE', #6679, .T. ) ;
#7057 = CARTESIAN_POINT ( 'NONE',  ( -18.05918829504999934, 10.97290950744599947, 63.54999999999999716 ) ) ;
#7058 = ORIENTED_EDGE ( 'NONE', *, *, #669, .F. ) ;
#7059 = AXIS2_PLACEMENT_3D ( 'NONE', #12785, #9575, #3503 ) ;
#7060 = CARTESIAN_POINT ( 'NONE',  ( -8.964285665223000521, 0.3335619008453594714, 62.14999999999999858 ) ) ;
#7061 = DIRECTION ( 'NONE',  ( 0.000000000000000000, 0.000000000000000000, 1.000000000000000000 ) ) ;
#7062 = CARTESIAN_POINT ( 'NONE',  ( -24.35918829505000005, 10.97290950744599947, 61.86500000000000199 ) ) ;
#7063 = ADVANCED_FACE ( 'NONE', ( #5309 ), #13634, .F. ) ;
#7064 = LINE ( 'NONE', #11339, #12948 ) ;
#7065 = ADVANCED_FACE ( 'NONE', ( #12733 ), #8458, .T. ) ;
#7066 = AXIS2_PLACEMENT_3D ( 'NONE', #7496, #6407, #10888 ) ;
#7067 = EDGE_CURVE ( 'NONE', #2183, #4982, #9580, .T. ) ;
#7068 = ORIENTED_EDGE ( 'NONE', *, *, #8106, .F. ) ;
#7069 = DIRECTION ( 'NONE',  ( -1.000000000000000000, 0.000000000000000000, 0.000000000000000000 ) ) ;
#7070 = CARTESIAN_POINT ( 'NONE',  ( -18.88608202933837177, 30.34555471844934615, 61.60507349188181081 ) ) ;
#7071 = CONICAL_SURFACE ( 'NONE', #8416, 4.250000000000000000, 0.7853981633974524978 ) ;
#7072 = CARTESIAN_POINT ( 'NONE',  ( 50.63563590245420443, 89.90549801902423610, 20.00000000000000000 ) ) ;
#7073 = CONICAL_SURFACE ( 'NONE', #8874, 6.145833333000002341, 0.2014252309328122270 ) ;
#7074 = DIRECTION ( 'NONE',  ( 1.000000000000000000, 0.000000000000000000, 0.000000000000000000 ) ) ;
#7075 = DIRECTION ( 'NONE',  ( 1.000000000000000000, 0.000000000000000000, 0.000000000000000000 ) ) ;
#7076 = AXIS2_PLACEMENT_3D ( 'NONE', #10657, #1085, #41 ) ;
#7077 = DIRECTION ( 'NONE',  ( -0.000000000000000000, 1.000000000000000000, -0.000000000000000000 ) ) ;
#7078 = DIRECTION ( 'NONE',  ( -0.1009684594134925978, 0.9948896271464819918, 0.000000000000000000 ) ) ;
#7079 = ORIENTED_EDGE ( 'NONE', *, *, #1566, .T. ) ;
#7080 = EDGE_CURVE ( 'NONE', #12066, #13005, #8479, .T. ) ;
#7081 = EDGE_CURVE ( 'NONE', #12302, #5689, #8714, .T. ) ;
#7082 = AXIS2_PLACEMENT_3D ( 'NONE', #6825, #7797, #12149 ) ;
#7083 = CIRCLE ( 'NONE', #12456, 1.500000000000001332 ) ;
#7084 = CARTESIAN_POINT ( 'NONE',  ( -25.67727386805000123, 10.97290950744599947, 61.65955166399999854 ) ) ;
#7085 = CARTESIAN_POINT ( 'NONE',  ( 50.63563590245420443, 89.90549801902423610, 22.89644660940672694 ) ) ;
#7086 = ORIENTED_EDGE ( 'NONE', *, *, #8673, .F. ) ;
#7087 = CARTESIAN_POINT ( 'NONE',  ( 0.09777679598749960954, -1.420146627243658033, 7.250000000000000000 ) ) ;
#7088 = DIRECTION ( 'NONE',  ( -8.673617379884027583E-16, 1.000000000000000000, -0.000000000000000000 ) ) ;
#7089 = CARTESIAN_POINT ( 'NONE',  ( 76.18094369249178044, 97.20665973629650125, 20.00000000000000000 ) ) ;
#7090 = CARTESIAN_POINT ( 'NONE',  ( 142.6356359024541973, 111.0390816101113245, 0.7500000000000006661 ) ) ;
#7091 = PLANE ( 'NONE',  #2912 ) ;
#7092 = DIRECTION ( 'NONE',  ( 1.000000000000000000, 0.000000000000000000, 0.000000000000000000 ) ) ;
#7093 = FACE_OUTER_BOUND ( 'NONE', #1962, .T. ) ;
#7094 = CARTESIAN_POINT ( 'NONE',  ( -25.86749127492454647, -8.860076549334129581, 17.25000000000000000 ) ) ;
#7095 = CARTESIAN_POINT ( 'NONE',  ( -18.05918829504999934, 10.97290950744599947, 67.84999999999999432 ) ) ;
#7096 = CIRCLE ( 'NONE', #2218, 9.999999999999994671 ) ;
#7097 = CIRCLE ( 'NONE', #9331, 1.999999999999991340 ) ;
#7098 = AXIS2_PLACEMENT_3D ( 'NONE', #8913, #2445, #261 ) ;
#7099 = CIRCLE ( 'NONE', #9112, 1.999999999999986233 ) ;
#7100 = PRODUCT_DEFINITION_CONTEXT ( 'detailed design', #6886, 'design' ) ;
#7101 = VERTEX_POINT ( 'NONE', #7450 ) ;
#7102 = VERTEX_POINT ( 'NONE', #13759 ) ;
#7103 = DIRECTION ( 'NONE',  ( -1.000000000000000000, 0.000000000000000000, 0.000000000000000000 ) ) ;
#7104 = EDGE_CURVE ( 'NONE', #11891, #11645, #12597, .T. ) ;
#7105 = ADVANCED_FACE ( 'NONE', ( #3045 ), #1344, .F. ) ;
#7106 = DIRECTION ( 'NONE',  ( -0.000000000000000000, -0.000000000000000000, 1.000000000000000000 ) ) ;
#7107 = VECTOR ( 'NONE', #1877, 1000.000000000000000 ) ;
#7108 = DIRECTION ( 'NONE',  ( -1.000000000000000000, 0.000000000000000000, 0.000000000000000000 ) ) ;
#7109 =( NAMED_UNIT ( * ) SI_UNIT ( $, .STERADIAN. ) SOLID_ANGLE_UNIT ( ) );
#7110 = DIRECTION ( 'NONE',  ( 0.000000000000000000, 0.000000000000000000, -1.000000000000000000 ) ) ;
#7111 = CARTESIAN_POINT ( 'NONE',  ( 134.8856359024541973, 94.65549801902425031, 23.00000000000000000 ) ) ;
#7112 = CARTESIAN_POINT ( 'NONE',  ( -11.74835982676941981, -4.028726038184999858, 62.14999999999999858 ) ) ;
#7113 = CONICAL_SURFACE ( 'NONE', #10914, 6.145833333000000565, 0.7853981633974503884 ) ;
#7114 = CIRCLE ( 'NONE', #4903, 33.00000000000000000 ) ;
#7115 = ORIENTED_EDGE ( 'NONE', *, *, #13565, .T. ) ;
#7116 = ORIENTED_EDGE ( 'NONE', *, *, #4784, .T. ) ;
#7117 = CARTESIAN_POINT ( 'NONE',  ( -14.30862101885204218, 30.05623439619531467, 58.39394286420760949 ) ) ;
#7118 = ORIENTED_EDGE ( 'NONE', *, *, #6132, .F. ) ;
#7119 = ORIENTED_EDGE ( 'NONE', *, *, #12786, .F. ) ;
#7120 = EDGE_CURVE ( 'NONE', #8048, #8866, #851, .T. ) ;
#7121 = ORIENTED_EDGE ( 'NONE', *, *, #767, .F. ) ;
#7122 = DIRECTION ( 'NONE',  ( -1.000000000000000000, 0.000000000000000000, 0.000000000000000000 ) ) ;
#7123 = CARTESIAN_POINT ( 'NONE',  ( -18.05918829504998513, 2.672909507137216867, 63.26715728756901314 ) ) ;
#7124 = EDGE_LOOP ( 'NONE', ( #4615, #11413, #5029, #8848 ) ) ;
#7125 = LINE ( 'NONE', #12447, #2219 ) ;
#7126 = CARTESIAN_POINT ( 'NONE',  ( 141.8856359024541973, 87.34974178189115435, 0.000000000000000000 ) ) ;
#7127 = ADVANCED_FACE ( 'NONE', ( #11742, #78 ), #11540, .F. ) ;
#7128 = DIRECTION ( 'NONE',  ( 1.000000000000000000, 0.000000000000000000, 0.000000000000000000 ) ) ;
#7129 = CIRCLE ( 'NONE', #4250, 4.250000000000000000 ) ;
#7130 = CARTESIAN_POINT ( 'NONE',  ( -35.05918829505000645, -6.027090492554000534, 17.25000000000000000 ) ) ;
#7131 = CONICAL_SURFACE ( 'NONE', #10056, 4.250000000000000000, 0.7853981633974524978 ) ;
#7132 = FACE_OUTER_BOUND ( 'NONE', #2453, .T. ) ;
#7133 = PRODUCT_RELATED_PRODUCT_CATEGORY ( 'part', '', ( #162 ) ) ;
#7134 = CARTESIAN_POINT ( 'NONE',  ( -4.059188295049996675, -6.027090492554000534, 0.000000000000000000 ) ) ;
#7135 = ADVANCED_FACE ( 'NONE', ( #6367, #8593 ), #4351, .T. ) ;
#7136 = ORIENTED_EDGE ( 'NONE', *, *, #6665, .T. ) ;
#7137 = VECTOR ( 'NONE', #1305, 1000.000000000000000 ) ;
#7138 = VECTOR ( 'NONE', #133, 1000.000000000000000 ) ;
#7139 = CIRCLE ( 'NONE', #6479, 5.500000000000000888 ) ;
#7140 = VECTOR ( 'NONE', #9859, 1000.000000000000114 ) ;
#7141 = EDGE_LOOP ( 'NONE', ( #6192, #9924, #4576, #6920 ) ) ;
#7142 = EDGE_CURVE ( 'NONE', #5559, #3451, #6152, .T. ) ;
#7143 = ORIENTED_EDGE ( 'NONE', *, *, #10617, .F. ) ;
#7144 = ORIENTED_EDGE ( 'NONE', *, *, #12034, .T. ) ;
#7145 = CARTESIAN_POINT ( 'NONE',  ( -4.499999999999999112, -0.5000000000000009992, -65.00000000000000000 ) ) ;
#7146 = CARTESIAN_POINT ( 'NONE',  ( -18.32176785559807541, 30.36027202460865482, 61.70913974837018401 ) ) ;
#7147 = DIRECTION ( 'NONE',  ( -0.9496839325805428444, -0.3132098788326364569, 0.000000000000000000 ) ) ;
#7148 = DIRECTION ( 'NONE',  ( 0.000000000000000000, 0.000000000000000000, 1.000000000000000000 ) ) ;
#7149 = DIRECTION ( 'NONE',  ( 0.000000000000000000, 0.000000000000000000, 1.000000000000000000 ) ) ;
#7150 = EDGE_CURVE ( 'NONE', #2952, #9710, #3107, .T. ) ;
#7151 = DIRECTION ( 'NONE',  ( 0.000000000000000000, 0.000000000000000000, -1.000000000000000000 ) ) ;
#7152 = CIRCLE ( 'NONE', #3822, 0.7500000000000006661 ) ;
#7153 = CARTESIAN_POINT ( 'NONE',  ( -20.55918829504999579, -23.02709049255400231, 94.85000000000000853 ) ) ;
#7154 = VECTOR ( 'NONE', #1644, 1000.000000000000000 ) ;
#7155 = EDGE_CURVE ( 'NONE', #7831, #6311, #4483, .T. ) ;
#7156 = STYLED_ITEM ( 'NONE', ( #4758 ), #4487 ) ;
#7157 = CARTESIAN_POINT ( 'NONE',  ( 140.3249757306743675, 112.2890816101113387, 0.000000000000000000 ) ) ;
#7158 = AXIS2_PLACEMENT_3D ( 'NONE', #11500, #2938, #7163 ) ;
#7159 = ORIENTED_EDGE ( 'NONE', *, *, #13532, .T. ) ;
#7160 = ORIENTED_EDGE ( 'NONE', *, *, #11090, .T. ) ;
#7161 = CARTESIAN_POINT ( 'NONE',  ( 141.8856359024541973, 87.34974178189115435, 20.00000000000000000 ) ) ;
#7162 = DIRECTION ( 'NONE',  ( 0.000000000000000000, 0.000000000000000000, -1.000000000000000000 ) ) ;
#7163 = DIRECTION ( 'NONE',  ( 0.000000000000000000, -0.000000000000000000, -1.000000000000000000 ) ) ;
#7164 = DIRECTION ( 'NONE',  ( -0.6615960714621569316, 0.7498604124941125049, 0.000000000000000000 ) ) ;
#7165 = DIRECTION ( 'NONE',  ( 0.000000000000000000, 0.000000000000000000, 1.000000000000000000 ) ) ;
#7166 = CARTESIAN_POINT ( 'NONE',  ( -18.05918829504999934, 10.97290950744599947, 57.35000000000000142 ) ) ;
#7167 = CYLINDRICAL_SURFACE ( 'NONE', #8044, 0.5000000000000000000 ) ;
#7168 = EDGE_CURVE ( 'NONE', #6678, #10600, #5242, .T. ) ;
#7169 = CARTESIAN_POINT ( 'NONE',  ( 0.000000000000000000, 0.000000000000000000, 0.000000000000000000 ) ) ;
#7170 = SURFACE_STYLE_USAGE ( .BOTH. , #9344 ) ;
#7171 = VERTEX_POINT ( 'NONE', #10002 ) ;
#7172 = ORIENTED_EDGE ( 'NONE', *, *, #8767, .F. ) ;
#7173 = ORIENTED_EDGE ( 'NONE', *, *, #7568, .T. ) ;
#7174 = DIRECTION ( 'NONE',  ( 0.000000000000000000, 0.000000000000000000, 1.000000000000000000 ) ) ;
#7175 = ORIENTED_EDGE ( 'NONE', *, *, #4060, .F. ) ;
#7176 = CARTESIAN_POINT ( 'NONE',  ( -20.45106689899080976, 15.53048109713862246, 68.70606566337372101 ) ) ;
#7177 = CIRCLE ( 'NONE', #7846, 16.66282263685194920 ) ;
#7178 = PLANE ( 'NONE',  #3372 ) ;
#7179 = FACE_OUTER_BOUND ( 'NONE', #13425, .T. ) ;
#7180 = CYLINDRICAL_SURFACE ( 'NONE', #11340, 4.750000000000000888 ) ;
#7181 = LINE ( 'NONE', #11459, #10709 ) ;
#7182 = ADVANCED_FACE ( 'NONE', ( #360 ), #7604, .T. ) ;
#7183 = VECTOR ( 'NONE', #312, 1000.000000000000114 ) ;
#7184 = ORIENTED_EDGE ( 'NONE', *, *, #4987, .F. ) ;
#7185 = CARTESIAN_POINT ( 'NONE',  ( -15.16757089999424402, 30.17981166147537309, 60.20239525771318512 ) ) ;
#7186 = ORIENTED_EDGE ( 'NONE', *, *, #3044, .F. ) ;
#7187 = DIRECTION ( 'NONE',  ( 0.000000000000000000, 0.000000000000000000, 1.000000000000000000 ) ) ;
#7188 = CARTESIAN_POINT ( 'NONE',  ( 3.940811704950003325, 35.97290950744599058, 10.00000000000000000 ) ) ;
#7189 = CARTESIAN_POINT ( 'NONE',  ( -18.05918829249644730, 2.672909507443099741, 63.15000000009349179 ) ) ;
#7190 = ORIENTED_EDGE ( 'NONE', *, *, #1133, .T. ) ;
#7191 = CARTESIAN_POINT ( 'NONE',  ( 98.63563590245422574, 99.03908161011133870, 0.000000000000000000 ) ) ;
#7192 = DIRECTION ( 'NONE',  ( -1.000000000000000000, 0.000000000000000000, 0.000000000000000000 ) ) ;
#7193 = ORIENTED_EDGE ( 'NONE', *, *, #12110, .T. ) ;
#7194 = DIRECTION ( 'NONE',  ( -0.000000000000000000, 1.000000000000000000, -0.000000000000000000 ) ) ;
#7195 = CIRCLE ( 'NONE', #9220, 1.999999999999994893 ) ;
#7196 = CARTESIAN_POINT ( 'NONE',  ( 185.2712718049083946, 94.65549801902425031, 23.00000000000000000 ) ) ;
#7197 = DIRECTION ( 'NONE',  ( 0.000000000000000000, 0.000000000000000000, -1.000000000000000000 ) ) ;
#7198 = PLANE ( 'NONE',  #4473 ) ;
#7199 = EDGE_CURVE ( 'NONE', #8025, #6125, #7669, .T. ) ;
#7200 = ORIENTED_EDGE ( 'NONE', *, *, #1698, .T. ) ;
#7201 = ADVANCED_FACE ( 'NONE', ( #9721 ), #8879, .T. ) ;
#7202 = AXIS2_PLACEMENT_3D ( 'NONE', #2536, #6767, #11039 ) ;
#7203 = ORIENTED_EDGE ( 'NONE', *, *, #8335, .F. ) ;
#7204 = ORIENTED_EDGE ( 'NONE', *, *, #820, .T. ) ;
#7205 = ORIENTED_EDGE ( 'NONE', *, *, #11671, .T. ) ;
#7206 = EDGE_LOOP ( 'NONE', ( #12111, #5246, #5519, #5081 ) ) ;
#7207 = CARTESIAN_POINT ( 'NONE',  ( -40.05918829505000645, 35.97290950744599058, 0.000000000000000000 ) ) ;
#7208 = DIRECTION ( 'NONE',  ( 1.000000000000000000, 0.000000000000000000, 0.000000000000000000 ) ) ;
#7209 = CYLINDRICAL_SURFACE ( 'NONE', #12345, 4.250000000000000000 ) ;
#7210 = CARTESIAN_POINT ( 'NONE',  ( -12.00000000000000000, -2.500000000000000444, 0.000000000000000000 ) ) ;
#7211 = FACE_OUTER_BOUND ( 'NONE', #5120, .T. ) ;
#7212 = DIRECTION ( 'NONE',  ( 1.000000000000000000, 0.000000000000000000, 0.000000000000000000 ) ) ;
#7213 = ADVANCED_FACE ( 'NONE', ( #9795, #10913, #6779, #11051, #1470, #9874, #4410, #6717 ), #13066, .T. ) ;
#7214 = AXIS2_PLACEMENT_3D ( 'NONE', #6173, #321, #11977 ) ;
#7215 = ORIENTED_EDGE ( 'NONE', *, *, #5516, .T. ) ;
#7216 = EDGE_CURVE ( 'NONE', #2266, #3627, #12095, .T. ) ;
#7217 = CARTESIAN_POINT ( 'NONE',  ( 140.6356359024541973, 113.0390816101113387, 0.7500000000000006661 ) ) ;
#7218 = DIRECTION ( 'NONE',  ( 1.000000000000000000, 0.000000000000000000, -0.000000000000000000 ) ) ;
#7219 = EDGE_LOOP ( 'NONE', ( #3702, #5314, #8340, #7277 ) ) ;
#7220 = CARTESIAN_POINT ( 'NONE',  ( 0.000000000000000000, 8.500000000000000000, 0.000000000000000000 ) ) ;
#7221 = CARTESIAN_POINT ( 'NONE',  ( -0.04028432657539302714, 4.500000000000000000, 16.54539866546729954 ) ) ;
#7222 = CARTESIAN_POINT ( 'NONE',  ( -23.05918829504999934, 10.97290950744599947, 116.8499999999999943 ) ) ;
#7223 = CARTESIAN_POINT ( 'NONE',  ( 16.08092853089229024, 0.000000000000000000, -9.237812082545193704 ) ) ;
#7224 = DIRECTION ( 'NONE',  ( 1.000000000000000000, 0.000000000000000000, -0.000000000000000000 ) ) ;
#7225 = CARTESIAN_POINT ( 'NONE',  ( 0.000000000000000000, 4.500000000000000000, 0.000000000000000000 ) ) ;
#7226 = CARTESIAN_POINT ( 'NONE',  ( -10.25088531517539714, 30.80589556422609832, 17.25000000000000000 ) ) ;
#7227 = DIRECTION ( 'NONE',  ( 1.000000000000000000, 0.000000000000000000, 0.000000000000000000 ) ) ;
#7228 = DIRECTION ( 'NONE',  ( -0.000000000000000000, 1.000000000000000000, -0.000000000000000000 ) ) ;
#7229 = EDGE_CURVE ( 'NONE', #9144, #3017, #1192, .T. ) ;
#7230 = AXIS2_PLACEMENT_3D ( 'NONE', #12317, #1618, #13217 ) ;
#7231 = ORIENTED_EDGE ( 'NONE', *, *, #6900, .T. ) ;
#7232 = EDGE_CURVE ( 'NONE', #10781, #1636, #7139, .T. ) ;
#7233 = CARTESIAN_POINT ( 'NONE',  ( 44.63563590245420443, 89.90549801902423610, 22.75000000000000000 ) ) ;
#7234 = ORIENTED_EDGE ( 'NONE', *, *, #7880, .F. ) ;
#7235 = EDGE_LOOP ( 'NONE', ( #8655, #2007, #22, #8672, #9573 ) ) ;
#7236 = VERTEX_POINT ( 'NONE', #213 ) ;
#7237 = CARTESIAN_POINT ( 'NONE',  ( -11.74835982676941981, -4.028726038184999858, 63.45000000000000284 ) ) ;
#7238 = CARTESIAN_POINT ( 'NONE',  ( 140.3249757306743675, 85.78908161011133870, 0.000000000000000000 ) ) ;
#7239 = ORIENTED_EDGE ( 'NONE', *, *, #12693, .T. ) ;
#7240 = CARTESIAN_POINT ( 'NONE',  ( -6.000000000000000888, 7.347880794884120722E-16, 7.000000000000000000 ) ) ;
#7241 = AXIS2_PLACEMENT_3D ( 'NONE', #3342, #4327, #2314 ) ;
#7242 = CARTESIAN_POINT ( 'NONE',  ( -3.499999999999998224, 2.000000000000000000, -65.00000000000000000 ) ) ;
#7243 = VERTEX_POINT ( 'NONE', #2413 ) ;
#7244 = VECTOR ( 'NONE', #11764, 1000.000000000000000 ) ;
#7245 = EDGE_CURVE ( 'NONE', #7236, #8398, #1332, .T. ) ;
#7246 = CARTESIAN_POINT ( 'NONE',  ( -14.93697936199538034, 30.14955231555997273, 59.86459082872807613 ) ) ;
#7247 = ORIENTED_EDGE ( 'NONE', *, *, #13338, .F. ) ;
#7248 = VERTEX_POINT ( 'NONE', #4698 ) ;
#7249 = DIRECTION ( 'NONE',  ( 1.000000000000000000, 0.000000000000000000, 0.000000000000000000 ) ) ;
#7250 = DIRECTION ( 'NONE',  ( 0.000000000000000000, 0.000000000000000000, -1.000000000000000000 ) ) ;
#7251 = DIRECTION ( 'NONE',  ( 0.000000000000000000, 0.000000000000000000, 1.000000000000000000 ) ) ;
#7252 = ORIENTED_EDGE ( 'NONE', *, *, #1410, .F. ) ;
#7253 = CYLINDRICAL_SURFACE ( 'NONE', #6868, 24.92993838181874722 ) ;
#7254 = DIRECTION ( 'NONE',  ( 0.000000000000000000, 0.000000000000000000, 1.000000000000000000 ) ) ;
#7255 = EDGE_LOOP ( 'NONE', ( #7003, #10074, #13200, #6772 ) ) ;
#7256 = FACE_OUTER_BOUND ( 'NONE', #4566, .T. ) ;
#7257 = CARTESIAN_POINT ( 'NONE',  ( -18.05918829504999934, 10.97290950744599947, 68.84999999999999432 ) ) ;
#7258 = DIRECTION ( 'NONE',  ( 0.000000000000000000, 0.000000000000000000, 1.000000000000000000 ) ) ;
#7259 = VECTOR ( 'NONE', #10622, 1000.000000000000000 ) ;
#7260 = CARTESIAN_POINT ( 'NONE',  ( -6.000000000000000888, 11.99999999999999822, 0.000000000000000000 ) ) ;
#7261 = EDGE_LOOP ( 'NONE', ( #3862, #10431 ) ) ;
#7262 = VERTEX_POINT ( 'NONE', #5588 ) ;
#7263 = ORIENTED_EDGE ( 'NONE', *, *, #10027, .F. ) ;
#7264 = ORIENTED_EDGE ( 'NONE', *, *, #10617, .T. ) ;
#7265 = CIRCLE ( 'NONE', #4838, 0.9499999999999995115 ) ;
#7266 = EDGE_CURVE ( 'NONE', #4150, #6531, #3586, .T. ) ;
#7267 = FACE_OUTER_BOUND ( 'NONE', #10886, .T. ) ;
#7268 = EDGE_CURVE ( 'NONE', #4017, #2836, #3510, .T. ) ;
#7269 = DIRECTION ( 'NONE',  ( 1.000000000000000000, 0.000000000000000000, 0.000000000000000000 ) ) ;
#7270 = CARTESIAN_POINT ( 'NONE',  ( -18.91658168612351787, 30.34444651895818268, 61.59715132800811688 ) ) ;
#7271 = CARTESIAN_POINT ( 'NONE',  ( 0.000000000000000000, 0.000000000000000000, 0.000000000000000000 ) ) ;
#7272 = DIRECTION ( 'NONE',  ( -0.000000000000000000, -0.000000000000000000, 1.000000000000000000 ) ) ;
#7273 = DIRECTION ( 'NONE',  ( -0.000000000000000000, -0.000000000000000000, 1.000000000000000000 ) ) ;
#7274 = FACE_OUTER_BOUND ( 'NONE', #2420, .T. ) ;
#7275 = ORIENTED_EDGE ( 'NONE', *, *, #13758, .T. ) ;
#7276 = VECTOR ( 'NONE', #8996, 1000.000000000000000 ) ;
#7277 = ORIENTED_EDGE ( 'NONE', *, *, #5327, .F. ) ;
#7278 = CARTESIAN_POINT ( 'NONE',  ( 140.6356359024541973, 113.0390816101113387, 19.68933982822018081 ) ) ;
#7279 = CARTESIAN_POINT ( 'NONE',  ( 0.04028432657539327000, 0.000000000000000000, -16.54539866546730309 ) ) ;
#7280 = ORIENTED_EDGE ( 'NONE', *, *, #1227, .T. ) ;
#7281 = DIRECTION ( 'NONE',  ( 0.000000000000000000, 0.000000000000000000, 1.000000000000000000 ) ) ;
#7282 = ADVANCED_FACE ( 'NONE', ( #3654 ), #8664, .F. ) ;
#7283 = DIRECTION ( 'NONE',  ( 0.000000000000000000, -1.000000000000000000, 0.000000000000000000 ) ) ;
#7284 = AXIS2_PLACEMENT_3D ( 'NONE', #13026, #11979, #6871 ) ;
#7285 = CARTESIAN_POINT ( 'NONE',  ( 82.99521369064696330, 82.14063840035363739, 20.00000000000000000 ) ) ;
#7286 = CARTESIAN_POINT ( 'NONE',  ( -4.599650328638321461, 8.500000000000000000, -7.878124499050794149 ) ) ;
#7287 = EDGE_LOOP ( 'NONE', ( #7115, #6332 ) ) ;
#7288 = FACE_OUTER_BOUND ( 'NONE', #6213, .T. ) ;
#7289 = CARTESIAN_POINT ( 'NONE',  ( 4.000000000000001776, 2.000000000000000000, -65.00000000000000000 ) ) ;
#7290 = DIRECTION ( 'NONE',  ( 1.000000000000000000, 0.000000000000000000, 0.000000000000000000 ) ) ;
#7291 = CARTESIAN_POINT ( 'NONE',  ( -10.89307956596845983, 10.97290950744599947, 61.72253826518770836 ) ) ;
#7292 = AXIS2_PLACEMENT_3D ( 'NONE', #2046, #4129, #12711 ) ;
#7293 = AXIS2_PLACEMENT_3D ( 'NONE', #13250, #4598, #12000 ) ;
#7294 = VERTEX_POINT ( 'NONE', #4486 ) ;
#7295 = VECTOR ( 'NONE', #6580, 1000.000000000000000 ) ;
#7296 = VERTEX_POINT ( 'NONE', #11811 ) ;
#7297 = VERTEX_POINT ( 'NONE', #8742 ) ;
#7298 = DIRECTION ( 'NONE',  ( -8.673617379884027583E-16, 1.000000000000000000, 0.000000000000000000 ) ) ;
#7300 = ADVANCED_FACE ( 'NONE', ( #2275 ), #6510, .F. ) ;
#7299 = VERTEX_POINT ( 'NONE', #7745 ) ;
#7301 = CARTESIAN_POINT ( 'NONE',  ( -20.12305801176480813, 15.81988081417610381, 68.58194257568855789 ) ) ;
#7302 = ORIENTED_EDGE ( 'NONE', *, *, #11954, .T. ) ;
#7303 = CARTESIAN_POINT ( 'NONE',  ( -11.74835982676941981, -4.028726038184999858, 62.14999999999999858 ) ) ;
#7304 = AXIS2_PLACEMENT_3D ( 'NONE', #3766, #344, #12079 ) ;
#7305 = DIRECTION ( 'NONE',  ( 1.000000000000000000, 0.000000000000000000, 0.000000000000000000 ) ) ;
#7306 = VECTOR ( 'NONE', #12802, 1000.000000000000114 ) ;
#7307 = TOROIDAL_SURFACE ( 'NONE', #7082, 10.75000000000000000, 0.7500000000000000000 ) ;
#7308 = CARTESIAN_POINT ( 'NONE',  ( -25.73489962141544751, -4.139534227248430120, 57.54999999999999716 ) ) ;
#7309 = AXIS2_PLACEMENT_3D ( 'NONE', #9175, #12384, #11334 ) ;
#7310 = CARTESIAN_POINT ( 'NONE',  ( -25.29804148384604900, -2.574630058508220021, 62.14999999999999858 ) ) ;
#7311 = ADVANCED_FACE ( 'NONE', ( #11955 ), #12314, .F. ) ;
#7312 = ADVANCED_FACE ( 'NONE', ( #1881 ), #3322, .F. ) ;
#7313 = AXIS2_PLACEMENT_3D ( 'NONE', #10278, #12576, #1747 ) ;
#7314 = VECTOR ( 'NONE', #11438, 1000.000000000000000 ) ;
#7315 = EDGE_LOOP ( 'NONE', ( #13035, #1548, #12799, #2702 ) ) ;
#7316 = CARTESIAN_POINT ( 'NONE',  ( -14.83031415886561000, 30.13477816397302789, 59.68356427289636912 ) ) ;
#7317 = ORIENTED_EDGE ( 'NONE', *, *, #13300, .F. ) ;
#7318 = VERTEX_POINT ( 'NONE', #4900 ) ;
#7319 = EDGE_CURVE ( 'NONE', #1146, #1530, #6025, .T. ) ;
#7320 = CARTESIAN_POINT ( 'NONE',  ( -18.05918829504999934, 10.97290950744599947, 57.35000000000000142 ) ) ;
#7321 =( LENGTH_UNIT ( ) NAMED_UNIT ( * ) SI_UNIT ( .MILLI., .METRE. ) );
#7322 =( REPRESENTATION_RELATIONSHIP ('NONE','NONE', #11848, #5156 ) REPRESENTATION_RELATIONSHIP_WITH_TRANSFORMATION ( #8614 )SHAPE_REPRESENTATION_RELATIONSHIP( ) );
#7323 = DIRECTION ( 'NONE',  ( 0.000000000000000000, 0.000000000000000000, -1.000000000000000000 ) ) ;
#7324 = VERTEX_POINT ( 'NONE', #6980 ) ;
#7325 = PLANE ( 'NONE',  #12014 ) ;
#7326 = CARTESIAN_POINT ( 'NONE',  ( -35.05918829505000645, 10.97290950744599947, 57.35000000000000142 ) ) ;
#7327 = CARTESIAN_POINT ( 'NONE',  ( -35.05918829504999934, 10.97290950744600124, 14.00000000000000000 ) ) ;
#7328 = CARTESIAN_POINT ( 'NONE',  ( -1.433900126049995061, 19.28555359244599288, 63.26601075299999621 ) ) ;
#7329 = EDGE_CURVE ( 'NONE', #4150, #2636, #2613, .T. ) ;
#7330 = CARTESIAN_POINT ( 'NONE',  ( 140.6356359024541973, 108.9054980190242503, 23.00000000000000000 ) ) ;
#7331 = VECTOR ( 'NONE', #3336, 1000.000000000000000 ) ;
#7332 = ORIENTED_EDGE ( 'NONE', *, *, #12628, .T. ) ;
#7333 = EDGE_LOOP ( 'NONE', ( #7610, #12376, #2568, #1323 ) ) ;
#7334 = AXIS2_PLACEMENT_3D ( 'NONE', #12230, #3710, #3507 ) ;
#7335 = CONICAL_SURFACE ( 'NONE', #9149, 6.595833333000001630, 0.4098752297613067475 ) ;
#7336 = DIRECTION ( 'NONE',  ( 0.000000000000000000, -1.000000000000000000, 0.000000000000000000 ) ) ;
#7337 = CARTESIAN_POINT ( 'NONE',  ( 134.6356359024541973, 103.9054980190242361, 20.00000000000000000 ) ) ;
#7338 = CARTESIAN_POINT ( 'NONE',  ( -28.87730642030694028, 29.81324547859995278, 17.25000000000000000 ) ) ;
#7339 = CARTESIAN_POINT ( 'NONE',  ( -19.31260878079642751, 26.92505106486307298, 56.52244572334543449 ) ) ;
#7340 = CARTESIAN_POINT ( 'NONE',  ( -5.809188295050001116, 27.97290950744599769, 7.250000000000000000 ) ) ;
#7341 = CARTESIAN_POINT ( 'NONE',  ( 7.640422211807137209, 16.89844320975774750, 7.000000000000000000 ) ) ;
#7342 = CARTESIAN_POINT ( 'NONE',  ( 92.63563590245421153, 99.03908161011133870, 19.25000000000000000 ) ) ;
#7343 = CONTEXT_DEPENDENT_SHAPE_REPRESENTATION ( #473, #8579 ) ;
#7344 = CONICAL_SURFACE ( 'NONE', #6023, 6.595833333000001630, 0.4098752297613067475 ) ;
#7345 = CIRCLE ( 'NONE', #4472, 0.7500000000000000000 ) ;
#7346 = VECTOR ( 'NONE', #13209, 1000.000000000000000 ) ;
#7347 = AXIS2_PLACEMENT_3D ( 'NONE', #1315, #2464, #4396 ) ;
#7348 = ADVANCED_FACE ( 'NONE', ( #3922 ), #4965, .F. ) ;
#7349 = ORIENTED_EDGE ( 'NONE', *, *, #9102, .T. ) ;
#7350 = CARTESIAN_POINT ( 'NONE',  ( 140.3249757306743675, 112.2890816101113387, 20.00000000000000000 ) ) ;
#7351 = CYLINDRICAL_SURFACE ( 'NONE', #5554, 2.000000000000001776 ) ;
#7352 = ORIENTED_EDGE ( 'NONE', *, *, #5867, .T. ) ;
#7353 = DIRECTION ( 'NONE',  ( 0.000000000000000000, 0.5150380749100549327, 0.8571673007021118895 ) ) ;
#7354 = DIRECTION ( 'NONE',  ( -1.000000000000000000, 0.000000000000000000, 0.000000000000000000 ) ) ;
#7355 = DIRECTION ( 'NONE',  ( 1.000000000000000000, 0.000000000000000000, 0.000000000000000000 ) ) ;
#7356 = AXIS2_PLACEMENT_3D ( 'NONE', #9375, #3037, #7251 ) ;
#7357 = AXIS2_PLACEMENT_3D ( 'NONE', #7303, #3982, #13741 ) ;
#7358 = CARTESIAN_POINT ( 'NONE',  ( 7.640422211807137209, 16.89844320975774750, 0.000000000000000000 ) ) ;
#7359 = ORIENTED_EDGE ( 'NONE', *, *, #7229, .T. ) ;
#7360 = CARTESIAN_POINT ( 'NONE',  ( -30.32854245105399826, -5.598733283342819611, 7.250000000000000000 ) ) ;
#7361 = VECTOR ( 'NONE', #1944, 1000.000000000000000 ) ;
#7362 = CARTESIAN_POINT ( 'NONE',  ( -12.62505638257885998, 21.67198471784914915, 62.85000000000000142 ) ) ;
#7363 = LINE ( 'NONE', #3075, #2278 ) ;
#7364 = DIRECTION ( 'NONE',  ( 1.000000000000000000, 0.000000000000000000, 0.000000000000000000 ) ) ;
#7365 = ADVANCED_FACE ( 'NONE', ( #10212 ), #628, .T. ) ;
#7366 = ORIENTED_EDGE ( 'NONE', *, *, #6002, .F. ) ;
#7367 = VECTOR ( 'NONE', #13770, 1000.000000000000000 ) ;
#7368 = CIRCLE ( 'NONE', #11412, 24.04163056034261459 ) ;
#7369 = VERTEX_POINT ( 'NONE', #8032 ) ;
#7370 = LINE ( 'NONE', #4459, #6133 ) ;
#7371 = ORIENTED_EDGE ( 'NONE', *, *, #13715, .T. ) ;
#7372 = EDGE_LOOP ( 'NONE', ( #5178, #12764, #10523, #4957 ) ) ;
#7373 = ORIENTED_EDGE ( 'NONE', *, *, #7548, .T. ) ;
#7374 = EDGE_LOOP ( 'NONE', ( #13736, #4907, #10501, #13258 ) ) ;
#7375 = FACE_OUTER_BOUND ( 'NONE', #2649, .T. ) ;
#7376 = CARTESIAN_POINT ( 'NONE',  ( -14.08961186627706041, 6.473747032481329988, 31.09999999999999787 ) ) ;
#7377 = CARTESIAN_POINT ( 'NONE',  ( -11.91335496205000055, 10.97290950744599947, 60.60999999999999943 ) ) ;
#7378 = CARTESIAN_POINT ( 'NONE',  ( -16.01484020223730553, 6.108714422173897596, 68.57364943554455294 ) ) ;
#7379 = AXIS2_PLACEMENT_3D ( 'NONE', #13252, #1515, #1592 ) ;
#7380 = DIRECTION ( 'NONE',  ( -1.000000000000000000, 0.000000000000000000, 0.000000000000000000 ) ) ;
#7381 = EDGE_CURVE ( 'NONE', #3628, #2929, #12163, .T. ) ;
#7382 = ORIENTED_EDGE ( 'NONE', *, *, #8126, .T. ) ;
#7383 = AXIS2_PLACEMENT_3D ( 'NONE', #7286, #13789, #1087 ) ;
#7384 = CYLINDRICAL_SURFACE ( 'NONE', #5896, 18.00000000000000000 ) ;
#7385 = EDGE_LOOP ( 'NONE', ( #9699, #6106 ) ) ;
#7386 = ORIENTED_EDGE ( 'NONE', *, *, #6001, .F. ) ;
#7387 = EDGE_LOOP ( 'NONE', ( #5784, #12588, #6710, #10607 ) ) ;
#7388 = LINE ( 'NONE', #1902, #9512 ) ;
#7389 = EDGE_CURVE ( 'NONE', #8708, #8341, #9936, .T. ) ;
#7390 = EDGE_CURVE ( 'NONE', #13422, #5137, #2144, .T. ) ;
#7391 = CARTESIAN_POINT ( 'NONE',  ( 134.6356359024541973, 94.90549801902425031, 20.00000000000000000 ) ) ;
#7392 = CARTESIAN_POINT ( 'NONE',  ( 76.11748380738829667, 115.4601262030644762, 0.000000000000000000 ) ) ;
#7393 = CARTESIAN_POINT ( 'NONE',  ( -9.143292286380720668, 6.444466247053390440, 64.85000000000000853 ) ) ;
#7394 = LINE ( 'NONE', #11810, #1320 ) ;
#7395 = CARTESIAN_POINT ( 'NONE',  ( -41.50918829505000218, 27.97290950744599769, 17.25000000000000000 ) ) ;
#7396 = AXIS2_PLACEMENT_3D ( 'NONE', #10644, #5324, #8472 ) ;
#7397 = ADVANCED_FACE ( 'NONE', ( #11187 ), #13488, .T. ) ;
#7398 = ORIENTED_EDGE ( 'NONE', *, *, #3531, .F. ) ;
#7399 = EDGE_LOOP ( 'NONE', ( #11945, #3158, #9148, #8568 ) ) ;
#7400 = VERTEX_POINT ( 'NONE', #9077 ) ;
#7401 = ORIENTED_EDGE ( 'NONE', *, *, #3002, .F. ) ;
#7402 = ORIENTED_EDGE ( 'NONE', *, *, #4608, .F. ) ;
#7403 = EDGE_CURVE ( 'NONE', #10469, #7611, #9037, .T. ) ;
#7404 = AXIS2_PLACEMENT_3D ( 'NONE', #11830, #13013, #13081 ) ;
#7405 = ORIENTED_EDGE ( 'NONE', *, *, #4901, .T. ) ;
#7406 = CARTESIAN_POINT ( 'NONE',  ( -25.33503448090910126, 29.19143287883919768, 64.85000000000000853 ) ) ;
#7407 = DIRECTION ( 'NONE',  ( -0.000000000000000000, -1.000000000000000000, -0.000000000000000000 ) ) ;
#7408 = CARTESIAN_POINT ( 'NONE',  ( -12.54628844161313950, -7.366404416634599883, 62.14999999999999858 ) ) ;
#7409 = CARTESIAN_POINT ( 'NONE',  ( -18.97262203685356141, 26.94685435944512264, 56.15999655357090603 ) ) ;
#7410 = CARTESIAN_POINT ( 'NONE',  ( -16.08092853089235774, 0.000000000000000000, 9.237812082545083570 ) ) ;
#7411 = DIRECTION ( 'NONE',  ( -1.000000000000000000, 0.000000000000000000, 0.000000000000000000 ) ) ;
#7412 = DIRECTION ( 'NONE',  ( 1.000000000000000000, 0.000000000000000000, 0.000000000000000000 ) ) ;
#7413 = VECTOR ( 'NONE', #13525, 1000.000000000000000 ) ;
#7414 = ORIENTED_EDGE ( 'NONE', *, *, #584, .T. ) ;
#7415 = ORIENTED_EDGE ( 'NONE', *, *, #3910, .T. ) ;
#7416 = EDGE_CURVE ( 'NONE', #3005, #6052, #13053, .T. ) ;
#7417 = CARTESIAN_POINT ( 'NONE',  ( 1.629816981350590055, -4.941769416738769571, 5.250000000000000000 ) ) ;
#7418 = ORIENTED_EDGE ( 'NONE', *, *, #3948, .F. ) ;
#7419 = FACE_OUTER_BOUND ( 'NONE', #11705, .T. ) ;
#7420 = CARTESIAN_POINT ( 'NONE',  ( 8.814269998155230823, -15.06602133594279991, -3.000000000000000000 ) ) ;
#7421 = DIRECTION ( 'NONE',  ( -0.7071067811865520136, 0.7071067811865429098, 0.000000000000000000 ) ) ;
#7422 = CARTESIAN_POINT ( 'NONE',  ( -20.55028075881694249, 30.22631440511032963, 54.04780568389777073 ) ) ;
#7423 = CARTESIAN_POINT ( 'NONE',  ( 140.3856359024541973, 0.000000000000000000, 22.75000000000000000 ) ) ;
#7424 = ORIENTED_EDGE ( 'NONE', *, *, #11445, .T. ) ;
#7425 = CARTESIAN_POINT ( 'NONE',  ( -2.819094421049990640, 18.59295644444599915, 61.63595870799996845 ) ) ;
#7426 = DIRECTION ( 'NONE',  ( 0.000000000000000000, 1.000000000000000000, 0.000000000000000000 ) ) ;
#7427 = CARTESIAN_POINT ( 'NONE',  ( -18.05918829505000289, 18.55161869500264515, 61.95399527332316580 ) ) ;
#7428 = DIRECTION ( 'NONE',  ( 0.000000000000000000, 0.000000000000000000, 1.000000000000000000 ) ) ;
#7429 = ORIENTED_EDGE ( 'NONE', *, *, #11318, .F. ) ;
#7430 = CARTESIAN_POINT ( 'NONE',  ( -18.05918829504999934, 10.97290950744599947, 62.85000000000000142 ) ) ;
#7431 = ORIENTED_EDGE ( 'NONE', *, *, #13603, .F. ) ;
#7432 = CARTESIAN_POINT ( 'NONE',  ( -7.241070169793070832, 29.81324547859995278, 17.25000000000000000 ) ) ;
#7433 = CARTESIAN_POINT ( 'NONE',  ( -28.87730642030695094, -7.867426463707980488, 17.25000000000000000 ) ) ;
#7434 = VERTEX_POINT ( 'NONE', #7891 ) ;
#7435 = PRESENTATION_STYLE_ASSIGNMENT (( #3351 ) ) ;
#7436 = EDGE_CURVE ( 'NONE', #7790, #13237, #3471, .T. ) ;
#7437 = DIRECTION ( 'NONE',  ( 1.000000000000000000, 0.000000000000000000, 0.000000000000000000 ) ) ;
#7438 = EDGE_CURVE ( 'NONE', #6850, #3038, #6120, .T. ) ;
#7439 = LINE ( 'NONE', #10613, #177 ) ;
#7440 = AXIS2_PLACEMENT_3D ( 'NONE', #9231, #13483, #12435 ) ;
#7441 = PRODUCT_RELATED_PRODUCT_CATEGORY ( 'part', '', ( #463 ) ) ;
#7442 = CARTESIAN_POINT ( 'NONE',  ( -16.48613393974217090, 30.30694957908812270, 53.37988226775320300 ) ) ;
#7443 = VECTOR ( 'NONE', #4259, 1000.000000000000000 ) ;
#7444 = CYLINDRICAL_SURFACE ( 'NONE', #10283, 6.449999999999997513 ) ;
#7445 = CARTESIAN_POINT ( 'NONE',  ( -10.25088531517539892, 30.80589556422609832, 17.25000000000000000 ) ) ;
#7446 = DIRECTION ( 'NONE',  ( 0.000000000000000000, 0.000000000000000000, -1.000000000000000000 ) ) ;
#7447 = CARTESIAN_POINT ( 'NONE',  ( -18.05918829504999934, 14.81548537210212046, 17.25000000000000000 ) ) ;
#7448 = EDGE_CURVE ( 'NONE', #7735, #10798, #10163, .T. ) ;
#7449 = CARTESIAN_POINT ( 'NONE',  ( -35.72201093190194854, 10.97290950744599947, 6.250000000000000000 ) ) ;
#7450 = CARTESIAN_POINT ( 'NONE',  ( -9.663354962050000552, 10.97290950744599947, 60.04999999999999716 ) ) ;
#7451 = EDGE_CURVE ( 'NONE', #6, #5283, #11710, .T. ) ;
#7452 = VECTOR ( 'NONE', #8843, 1000.000000000000000 ) ;
#7453 = ADVANCED_FACE ( 'NONE', ( #8812 ), #1262, .T. ) ;
#7454 = ORIENTED_EDGE ( 'NONE', *, *, #736, .T. ) ;
#7455 = CYLINDRICAL_SURFACE ( 'NONE', #2586, 17.00000000000000000 ) ;
#7456 = ORIENTED_EDGE ( 'NONE', *, *, #2366, .T. ) ;
#7457 = ORIENTED_EDGE ( 'NONE', *, *, #9180, .T. ) ;
#7458 = VERTEX_POINT ( 'NONE', #3514 ) ;
#7459 = DIRECTION ( 'NONE',  ( 0.000000000000000000, 0.000000000000000000, 1.000000000000000000 ) ) ;
#7460 = FACE_OUTER_BOUND ( 'NONE', #11214, .T. ) ;
#7461 = ADVANCED_FACE ( 'NONE', ( #8671 ), #4294, .F. ) ;
#7462 = EDGE_LOOP ( 'NONE', ( #1363, #9847 ) ) ;
#7463 = AXIS2_PLACEMENT_3D ( 'NONE', #13380, #10449, #9413 ) ;
#7464 = DIRECTION ( 'NONE',  ( -1.000000000000000000, 0.000000000000000000, 0.000000000000000000 ) ) ;
#7465 = DIRECTION ( 'NONE',  ( 0.000000000000000000, 0.000000000000000000, 1.000000000000000000 ) ) ;
#7466 = CARTESIAN_POINT ( 'NONE',  ( 140.6356359024541689, 85.78908161011133870, 20.00000000000000000 ) ) ;
#7467 = CARTESIAN_POINT ( 'NONE',  ( -12.00918829504999863, 10.97290950744599947, 0.000000000000000000 ) ) ;
#7468 = EDGE_CURVE ( 'NONE', #12568, #54, #8600, .T. ) ;
#7469 = LINE ( 'NONE', #11760, #451 ) ;
#7470 = ADVANCED_FACE ( 'NONE', ( #81 ), #10848, .T. ) ;
#7471 = CIRCLE ( 'NONE', #800, 34.70000000000000284 ) ;
#7472 = VERTEX_POINT ( 'NONE', #9663 ) ;
#7473 = ORIENTED_EDGE ( 'NONE', *, *, #13512, .F. ) ;
#7474 = DIRECTION ( 'NONE',  ( 0.000000000000000000, 0.000000000000000000, 1.000000000000000000 ) ) ;
#7475 = ORIENTED_EDGE ( 'NONE', *, *, #13300, .T. ) ;
#7476 = DIRECTION ( 'NONE',  ( -0.000000000000000000, -0.000000000000000000, -1.000000000000000000 ) ) ;
#7477 = DIRECTION ( 'NONE',  ( 0.2878798879079290662, 0.9576665234506832602, 0.000000000000000000 ) ) ;
#7478 = DIRECTION ( 'NONE',  ( 0.000000000000000000, 0.000000000000000000, 1.000000000000000000 ) ) ;
#7479 = CARTESIAN_POINT ( 'NONE',  ( -20.69640587970463486, 30.21012672718795855, 54.19793656979756236 ) ) ;
#7480 = CARTESIAN_POINT ( 'NONE',  ( 0.000000000000000000, 8.500000000000000000, 6.000000000000000888 ) ) ;
#7481 = ORIENTED_EDGE ( 'NONE', *, *, #5350, .F. ) ;
#7482 = DIRECTION ( 'NONE',  ( 0.000000000000000000, 0.000000000000000000, -1.000000000000000000 ) ) ;
#7483 = DIRECTION ( 'NONE',  ( -1.000000000000000000, 0.000000000000000000, 0.000000000000000000 ) ) ;
#7484 = PLANE ( 'NONE',  #9621 ) ;
#7485 = CIRCLE ( 'NONE', #11087, 2.000000000000001776 ) ;
#7486 = CARTESIAN_POINT ( 'NONE',  ( -27.49999999999998934, 9.000000000000000000, 29.99999999999999645 ) ) ;
#7487 =( NAMED_UNIT ( * ) PLANE_ANGLE_UNIT ( ) SI_UNIT ( $, .RADIAN. ) );
#7488 = EDGE_CURVE ( 'NONE', #5579, #6589, #12818, .T. ) ;
#7489 = ORIENTED_EDGE ( 'NONE', *, *, #11105, .F. ) ;
#7490 = VECTOR ( 'NONE', #11295, 1000.000000000000000 ) ;
#7491 = ORIENTED_EDGE ( 'NONE', *, *, #10576, .F. ) ;
#7492 = CARTESIAN_POINT ( 'NONE',  ( -23.57208814848684852, -7.366404416634599883, 62.14999999999999858 ) ) ;
#7493 = ORIENTED_EDGE ( 'NONE', *, *, #511, .F. ) ;
#7494 = ORIENTED_EDGE ( 'NONE', *, *, #1282, .T. ) ;
#7495 = ORIENTED_EDGE ( 'NONE', *, *, #11585, .T. ) ;
#7496 = CARTESIAN_POINT ( 'NONE',  ( -18.45469220996244886, -1.832421873814834123, 7.000000000000000000 ) ) ;
#7497 = PRODUCT_DEFINITION_SHAPE ( 'NONE', 'NONE',  #738 ) ;
#7498 = DIRECTION ( 'NONE',  ( 1.000000000000000000, 0.000000000000000000, 0.000000000000000000 ) ) ;
#7499 = CARTESIAN_POINT ( 'NONE',  ( -18.05918829504999934, 10.97290950744599947, 5.250000000000000000 ) ) ;
#7500 = DIRECTION ( 'NONE',  ( 1.000000000000000000, 0.000000000000000000, 0.000000000000000000 ) ) ;
#7501 = CARTESIAN_POINT ( 'NONE',  ( 18.45469220996244886, 1.832421873814834123, 7.000000000000000000 ) ) ;
#7502 = DIRECTION ( 'NONE',  ( -0.6615960714621564875, 0.7498604124941129490, 0.000000000000000000 ) ) ;
#7503 = CIRCLE ( 'NONE', #11325, 0.7499999999999966693 ) ;
#7504 = CIRCLE ( 'NONE', #9323, 16.95000000000000284 ) ;
#7505 = VECTOR ( 'NONE', #7849, 1000.000000000000114 ) ;
#7506 = ADVANCED_FACE ( 'NONE', ( #2201 ), #12797, .T. ) ;
#7507 = ORIENTED_EDGE ( 'NONE', *, *, #1648, .F. ) ;
#7508 = EDGE_CURVE ( 'NONE', #8435, #4307, #6795, .T. ) ;
#7509 = CARTESIAN_POINT ( 'NONE',  ( 109.0903281124166710, 100.8715034839261762, 10.00000000000000000 ) ) ;
#7510 = AXIS2_PLACEMENT_3D ( 'NONE', #903, #10279, #8242 ) ;
#7511 = CIRCLE ( 'NONE', #4428, 1.999999999999991340 ) ;
#7512 = AXIS2_PLACEMENT_3D ( 'NONE', #4678, #8933, #13190 ) ;
#7513 = ORIENTED_EDGE ( 'NONE', *, *, #11023, .F. ) ;
#7514 = ORIENTED_EDGE ( 'NONE', *, *, #2906, .F. ) ;
#7515 = CARTESIAN_POINT ( 'NONE',  ( -10.79835982676942052, -4.028726038184999858, 62.14999999999999858 ) ) ;
#7516 = AXIS2_PLACEMENT_3D ( 'NONE', #1480, #8754, #1347 ) ;
#7517 = CARTESIAN_POINT ( 'NONE',  ( 16.08092853089229024, 0.000000000000000000, -9.237812082545193704 ) ) ;
#7518 = SURFACE_STYLE_FILL_AREA ( #11950 ) ;
#7519 = CARTESIAN_POINT ( 'NONE',  ( 111.0903281124166710, 100.8715034839261762, 10.00000000000000000 ) ) ;
#7520 = CARTESIAN_POINT ( 'NONE',  ( 68.49370948373500312, 112.2890816101113387, 0.000000000000000000 ) ) ;
#7521 = DIRECTION ( 'NONE',  ( 0.000000000000000000, 1.000000000000000000, -0.000000000000000000 ) ) ;
#7522 = DIRECTION ( 'NONE',  ( 0.000000000000000000, 0.000000000000000000, -1.000000000000000000 ) ) ;
#7523 = CIRCLE ( 'NONE', #11580, 16.72262947720610171 ) ;
#7524 = VECTOR ( 'NONE', #3506, 1000.000000000000114 ) ;
#7525 = VECTOR ( 'NONE', #10737, 1000.000000000000000 ) ;
#7526 = CIRCLE ( 'NONE', #2679, 1.999999999999996669 ) ;
#7527 = EDGE_LOOP ( 'NONE', ( #4988, #5482, #4460, #10028 ) ) ;
#7528 = ORIENTED_EDGE ( 'NONE', *, *, #9916, .F. ) ;
#7529 = ADVANCED_FACE ( 'NONE', ( #10706 ), #3449, .F. ) ;
#7530 = ORIENTED_EDGE ( 'NONE', *, *, #12273, .F. ) ;
#7531 =( BOUNDED_SURFACE ( )  B_SPLINE_SURFACE ( 3, 3, ( 
 ( #2374, #8624, #12961, #4450 ),
 ( #44, #105, #8776, #6598 ),
 ( #1088, #5548, #4379, #10808 ),
 ( #4522, #11773, #7425, #9751 ) ),
 .UNSPECIFIED., .F., .F., .T. ) 
 B_SPLINE_SURFACE_WITH_KNOTS ( ( 4, 4 ),
 ( 4, 4 ),
 ( 0.000000000000000000, 1.000000000000000000 ),
 ( 0.000000000000000000, 1.000000000000000000 ),
 .UNSPECIFIED. ) 
 GEOMETRIC_REPRESENTATION_ITEM ( )  RATIONAL_B_SPLINE_SURFACE ( (
 ( 1.000000000000000000, 0.3333333333333329818, 0.3333333333333329818, 1.000000000000000000),
 ( 0.4470472315060959878, 0.1490157438353659769, 0.1490157438353659769, 0.4470472315060959878),
 ( 0.4470472315060959878, 0.1490157438353659769, 0.1490157438353659769, 0.4470472315060959878),
 ( 1.000000000000000000, 0.3333333333333329818, 0.3333333333333329818, 1.000000000000000000) ) ) 
 REPRESENTATION_ITEM ( '' )  SURFACE ( )  );
#7532 = CARTESIAN_POINT ( 'NONE',  ( 0.000000000000000000, 4.500000000000000000, -13.50000000000000000 ) ) ;
#7533 = ORIENTED_EDGE ( 'NONE', *, *, #9078, .F. ) ;
#7534 = EDGE_LOOP ( 'NONE', ( #11890, #5656, #5479, #879 ) ) ;
#7535 = AXIS2_PLACEMENT_3D ( 'NONE', #7997, #12196, #5685 ) ;
#7536 = ORIENTED_EDGE ( 'NONE', *, *, #230, .T. ) ;
#7537 = FACE_OUTER_BOUND ( 'NONE', #12770, .T. ) ;
#7538 = CARTESIAN_POINT ( 'NONE',  ( -5.809188295050001116, 27.97290950744599769, 64.85000000000000853 ) ) ;
#7539 = ORIENTED_EDGE ( 'NONE', *, *, #8564, .T. ) ;
#7540 = CARTESIAN_POINT ( 'NONE',  ( 0.000000000000000000, 0.000000000000000000, 5.250000000000000000 ) ) ;
#7541 = AXIS2_PLACEMENT_3D ( 'NONE', #4622, #5511, #2341 ) ;
#7542 = LINE ( 'NONE', #8683, #6314 ) ;
#7543 = DIRECTION ( 'NONE',  ( 1.000000000000000000, 0.000000000000000000, 0.000000000000000000 ) ) ;
#7544 = AXIS2_PLACEMENT_3D ( 'NONE', #9744, #8417, #8693 ) ;
#7545 = CARTESIAN_POINT ( 'NONE',  ( -25.64433075620760150, -3.961216307075045240, 61.85000000000000142 ) ) ;
#7546 = DIRECTION ( 'NONE',  ( 1.000000000000000000, 0.000000000000000000, 0.000000000000000000 ) ) ;
#7547 = ORIENTED_EDGE ( 'NONE', *, *, #7548, .F. ) ;
#7548 = EDGE_CURVE ( 'NONE', #12198, #4364, #3902, .T. ) ;
#7549 = CIRCLE ( 'NONE', #3785, 1.999999999999993117 ) ;
#7550 = VECTOR ( 'NONE', #9755, 1000.000000000000114 ) ;
#7551 = ORIENTED_EDGE ( 'NONE', *, *, #3701, .F. ) ;
#7552 = ORIENTED_EDGE ( 'NONE', *, *, #12631, .T. ) ;
#7553 = ORIENTED_EDGE ( 'NONE', *, *, #4225, .T. ) ;
#7554 = DIRECTION ( 'NONE',  ( 0.000000000000000000, 0.000000000000000000, -1.000000000000000000 ) ) ;
#7555 = VERTEX_POINT ( 'NONE', #5315 ) ;
#7556 = LINE ( 'NONE', #10868, #11983 ) ;
#7557 = CARTESIAN_POINT ( 'NONE',  ( -18.05918829504999934, 10.97290950744599947, 30.59999999999999787 ) ) ;
#7558 = EDGE_CURVE ( 'NONE', #6706, #12630, #5446, .T. ) ;
#7559 = CARTESIAN_POINT ( 'NONE',  ( -18.05918829504999934, 30.36027202460864771, 52.99086025162979752 ) ) ;
#7560 = CARTESIAN_POINT ( 'NONE',  ( 86.63563590245421153, 99.03908161011133870, 0.000000000000000000 ) ) ;
#7561 = CARTESIAN_POINT ( 'NONE',  ( -18.05918829504999934, 10.97290950744599947, 62.14999999999999858 ) ) ;
#7562 = CARTESIAN_POINT ( 'NONE',  ( 16.08092853089229024, 0.000000000000000000, -11.23781208254518660 ) ) ;
#7563 = CARTESIAN_POINT ( 'NONE',  ( -4.499999999999999112, -0.5000000000000009992, -65.00000000000000000 ) ) ;
#7564 = DIRECTION ( 'NONE',  ( 0.000000000000000000, 0.000000000000000000, 1.000000000000000000 ) ) ;
#7565 = CIRCLE ( 'NONE', #13599, 6.749999999999999112 ) ;
#7566 = VECTOR ( 'NONE', #10695, 1000.000000000000000 ) ;
#7567 = AXIS2_PLACEMENT_3D ( 'NONE', #9528, #2289, #9470 ) ;
#7568 = EDGE_CURVE ( 'NONE', #12316, #10704, #5385, .T. ) ;
#7569 = ORIENTED_EDGE ( 'NONE', *, *, #12372, .T. ) ;
#7570 = ORIENTED_EDGE ( 'NONE', *, *, #12942, .T. ) ;
#7571 = ORIENTED_EDGE ( 'NONE', *, *, #11990, .F. ) ;
#7572 = VECTOR ( 'NONE', #7477, 1000.000000000000227 ) ;
#7573 = DIRECTION ( 'NONE',  ( 0.2878798879079290662, 0.9576665234506832602, 0.000000000000000000 ) ) ;
#7574 = ORIENTED_EDGE ( 'NONE', *, *, #6223, .F. ) ;
#7575 = AXIS2_PLACEMENT_3D ( 'NONE', #5841, #6822, #3634 ) ;
#7576 = AXIS2_PLACEMENT_3D ( 'NONE', #12794, #11615, #9658 ) ;
#7577 = AXIS2_PLACEMENT_3D ( 'NONE', #13559, #4840, #3873 ) ;
#7578 = ORIENTED_EDGE ( 'NONE', *, *, #1439, .T. ) ;
#7579 = EDGE_LOOP ( 'NONE', ( #7402, #8606 ) ) ;
#7580 = ORIENTED_EDGE ( 'NONE', *, *, #12866, .F. ) ;
#7581 = DIRECTION ( 'NONE',  ( -1.000000000000000000, -2.529805069132845816E-16, -0.000000000000000000 ) ) ;
#7582 = ADVANCED_FACE ( 'NONE', ( #3303 ), #7455, .F. ) ;
#7583 = DIRECTION ( 'NONE',  ( -1.000000000000000000, 0.000000000000000000, 0.000000000000000000 ) ) ;
#7584 = CARTESIAN_POINT ( 'NONE',  ( -1.059188295049996231, 27.97290950744599769, 58.85000000000000142 ) ) ;
#7585 = DIRECTION ( 'NONE',  ( -0.7071067811865451302, 0.7071067811865500152, -0.000000000000000000 ) ) ;
#7586 = FACE_OUTER_BOUND ( 'NONE', #4139, .T. ) ;
#7587 = CARTESIAN_POINT ( 'NONE',  ( -30.32854245105399826, 27.54455229823479812, 7.250000000000000000 ) ) ;
#7588 = CARTESIAN_POINT ( 'NONE',  ( -10.25088531517540069, -8.860076549334108265, 83.57661607529820458 ) ) ;
#7589 = VECTOR ( 'NONE', #6218, 1000.000000000000000 ) ;
#7590 = CONICAL_SURFACE ( 'NONE', #1584, 4.546599999999997976, 1.029744258676653645 ) ;
#7591 = VECTOR ( 'NONE', #9905, 1000.000000000000114 ) ;
#7592 = ORIENTED_EDGE ( 'NONE', *, *, #8942, .F. ) ;
#7593 = CARTESIAN_POINT ( 'NONE',  ( -16.42191933243140056, 30.30251685243779036, 53.41373514583168713 ) ) ;
#7594 = VERTEX_POINT ( 'NONE', #13072 ) ;
#7595 = CARTESIAN_POINT ( 'NONE',  ( -35.05918829505000645, 27.97290950744599769, 10.00000000000000000 ) ) ;
#7596 = COLOUR_RGB ( '', 0.40784314, 0.44705882, 0.49803922) ;
#7597 = DIRECTION ( 'NONE',  ( 0.000000000000000000, 0.000000000000000000, 1.000000000000000000 ) ) ;
#7598 = AXIS2_PLACEMENT_3D ( 'NONE', #11353, #13649, #10306 ) ;
#7599 = CIRCLE ( 'NONE', #10746, 0.7499999999999966693 ) ;
#7600 = ORIENTED_EDGE ( 'NONE', *, *, #8564, .F. ) ;
#7601 = DIRECTION ( 'NONE',  ( -1.000000000000000000, 0.000000000000000000, 0.000000000000000000 ) ) ;
#7602 = CARTESIAN_POINT ( 'NONE',  ( 75.58559257550551536, 115.9888905337886769, 20.00000000000000000 ) ) ;
#7603 = EDGE_CURVE ( 'NONE', #12804, #6443, #12607, .T. ) ;
#7604 = CYLINDRICAL_SURFACE ( 'NONE', #12729, 34.69999999999999574 ) ;
#7605 = AXIS2_PLACEMENT_3D ( 'NONE', #7499, #4334, #9562 ) ;
#7606 = ORIENTED_EDGE ( 'NONE', *, *, #10444, .F. ) ;
#7607 = EDGE_LOOP ( 'NONE', ( #699, #6059, #4557, #6371 ) ) ;
#7608 = ORIENTED_EDGE ( 'NONE', *, *, #10133, .F. ) ;
#7609 = CARTESIAN_POINT ( 'NONE',  ( 50.38563590245420443, 0.000000000000000000, 23.00000000000000000 ) ) ;
#7610 = ORIENTED_EDGE ( 'NONE', *, *, #13673, .F. ) ;
#7611 = VERTEX_POINT ( 'NONE', #7532 ) ;
#7612 = VERTEX_POINT ( 'NONE', #11820 ) ;
#7613 = DIRECTION ( 'NONE',  ( -0.7071067811865425767, 0.7071067811865524577, 0.000000000000000000 ) ) ;
#7614 = DIRECTION ( 'NONE',  ( 0.000000000000000000, -1.000000000000000000, 2.732534507816519619E-15 ) ) ;
#7615 = ORIENTED_EDGE ( 'NONE', *, *, #11566, .F. ) ;
#7616 = CARTESIAN_POINT ( 'NONE',  ( -1.396365658198039927, 10.97290950744599947, 5.250000000000000000 ) ) ;
#7617 = STYLED_ITEM ( 'NONE', ( #3207 ), #5147 ) ;
#7618 = CARTESIAN_POINT ( 'NONE',  ( -16.68844204839930612, 26.91524980442654069, 56.72172238493448049 ) ) ;
#7619 = EDGE_CURVE ( 'NONE', #10997, #10707, #10964, .T. ) ;
#7620 = CARTESIAN_POINT ( 'NONE',  ( -38.38077571930825371, 22.44393519180574970, 17.25000000000000000 ) ) ;
#7621 = DIRECTION ( 'NONE',  ( 0.000000000000000000, 0.000000000000000000, -1.000000000000000000 ) ) ;
#7622 = EDGE_CURVE ( 'NONE', #9965, #1818, #6513, .T. ) ;
#7623 = DIRECTION ( 'NONE',  ( -1.000000000000000000, 0.000000000000000000, 0.000000000000000000 ) ) ;
#7624 = CONTEXT_DEPENDENT_SHAPE_REPRESENTATION ( #11010, #4251 ) ;
#7625 =( BOUNDED_CURVE ( )  B_SPLINE_CURVE ( 3, ( #2860, #7085, #11364, #9539 ),
 .UNSPECIFIED., .F., .F. ) 
 B_SPLINE_CURVE_WITH_KNOTS ( ( 4, 4 ),
 ( 0.000000000000000000, 1.570796326794896558 ),
 .UNSPECIFIED. ) 
 CURVE ( )  GEOMETRIC_REPRESENTATION_ITEM ( )  RATIONAL_B_SPLINE_CURVE ( ( 1.000000000000000000, 0.8047378541243649375, 0.8047378541243649375, 1.000000000000000000 ) ) 
 REPRESENTATION_ITEM ( '' )  );
#7626 = ORIENTED_EDGE ( 'NONE', *, *, #2816, .F. ) ;
#7627 = COLOUR_RGB ( '', 0.31764706, 0.68627451, 0.89019608) ;
#7628 = PRODUCT ( 'Flange', 'Flange', '', ( #4101 ) ) ;
#7629 = EDGE_CURVE ( 'NONE', #6571, #2036, #2764, .T. ) ;
#7630 = EDGE_LOOP ( 'NONE', ( #2315, #12917, #3145, #2469 ) ) ;
#7631 = EDGE_LOOP ( 'NONE', ( #4062, #12220 ) ) ;
#7632 = CARTESIAN_POINT ( 'NONE',  ( -11.74835982676941981, -4.028726038184999858, 62.14999999999999858 ) ) ;
#7633 = FACE_BOUND ( 'NONE', #13054, .T. ) ;
#7634 = DIRECTION ( 'NONE',  ( 0.000000000000000000, 0.000000000000000000, -1.000000000000000000 ) ) ;
#7635 = FILL_AREA_STYLE_COLOUR ( '', #1278 ) ;
#7636 = CARTESIAN_POINT ( 'NONE',  ( -18.19063477396443318, 30.36027202460863705, 52.99086025162979752 ) ) ;
#7637 = VERTEX_POINT ( 'NONE', #6782 ) ;
#7638 = DIRECTION ( 'NONE',  ( -0.7071067811865525687, -0.7071067811865425767, 0.000000000000000000 ) ) ;
#7639 = FACE_OUTER_BOUND ( 'NONE', #13157, .T. ) ;
#7640 = DIRECTION ( 'NONE',  ( 0.000000000000000000, 0.000000000000000000, 1.000000000000000000 ) ) ;
#7641 = EDGE_CURVE ( 'NONE', #2149, #380, #10372, .T. ) ;
#7642 = VECTOR ( 'NONE', #13632, 1000.000000000000114 ) ;
#7643 = DIRECTION ( 'NONE',  ( 0.000000000000000000, 1.000000000000000000, 0.000000000000000000 ) ) ;
#7644 = EDGE_CURVE ( 'NONE', #2345, #467, #6574, .T. ) ;
#7645 = EDGE_CURVE ( 'NONE', #11014, #2826, #13344, .T. ) ;
#7646 = ORIENTED_EDGE ( 'NONE', *, *, #5349, .F. ) ;
#7647 = EDGE_LOOP ( 'NONE', ( #4630, #6917 ) ) ;
#7648 = CIRCLE ( 'NONE', #4983, 1.999999999999991340 ) ;
#7649 = EDGE_LOOP ( 'NONE', ( #3771, #3093, #5866, #2041 ) ) ;
#7650 = CARTESIAN_POINT ( 'NONE',  ( 140.6356359024541973, 94.90549801902423610, 22.89644660940672694 ) ) ;
#7651 = CARTESIAN_POINT ( 'NONE',  ( -4.599650328638321461, 8.500000000000000000, -9.878124499050780827 ) ) ;
#7652 = DIRECTION ( 'NONE',  ( 0.000000000000000000, 0.000000000000000000, 1.000000000000000000 ) ) ;
#7653 = LINE ( 'NONE', #11935, #5513 ) ;
#7654 = CARTESIAN_POINT ( 'NONE',  ( -18.05918829504999934, 10.97290950744599947, 60.04999999999999716 ) ) ;
#7655 = FACE_BOUND ( 'NONE', #1339, .T. ) ;
#7656 = FACE_OUTER_BOUND ( 'NONE', #12441, .T. ) ;
#7657 = LINE ( 'NONE', #1173, #5574 ) ;
#7658 = EDGE_CURVE ( 'NONE', #6311, #7831, #4136, .T. ) ;
#7659 = CARTESIAN_POINT ( 'NONE',  ( -26.35918829505000005, 10.97290950744599947, 61.86500000000000199 ) ) ;
#7660 = DIRECTION ( 'NONE',  ( 0.000000000000000000, 0.000000000000000000, 1.000000000000000000 ) ) ;
#7661 = ADVANCED_FACE ( 'NONE', ( #9937 ), #8959, .F. ) ;
#7662 = ORIENTED_EDGE ( 'NONE', *, *, #10144, .T. ) ;
#7663 = CARTESIAN_POINT ( 'NONE',  ( -16.95433748440508737, 30.33404188113821931, 53.17780894285112225 ) ) ;
#7664 = ORIENTED_EDGE ( 'NONE', *, *, #12073, .T. ) ;
#7665 = DIRECTION ( 'NONE',  ( 0.000000000000000000, 0.000000000000000000, -1.000000000000000000 ) ) ;
#7666 = CARTESIAN_POINT ( 'NONE',  ( -12.54628844161313950, -7.366404416634599883, 62.14999999999999858 ) ) ;
#7667 = FACE_OUTER_BOUND ( 'NONE', #2955, .T. ) ;
#7668 = CARTESIAN_POINT ( 'NONE',  ( -18.05918829504999934, 19.27191034044600215, 63.13003331699999876 ) ) ;
#7669 = LINE ( 'NONE', #8956, #6262 ) ;
#7670 = ADVANCED_FACE ( 'NONE', ( #8037 ), #9708, .F. ) ;
#7671 = ADVANCED_FACE ( 'NONE', ( #4905 ), #13141, .F. ) ;
#7672 = EDGE_LOOP ( 'NONE', ( #2765, #11131, #9328, #7514 ) ) ;
#7673 = ORIENTED_EDGE ( 'NONE', *, *, #10444, .T. ) ;
#7674 = AXIS2_PLACEMENT_3D ( 'NONE', #11321, #1751, #4764 ) ;
#7675 = CARTESIAN_POINT ( 'NONE',  ( 141.8856359024541973, 110.7284214383315089, 20.00000000000000000 ) ) ;
#7676 = ORIENTED_EDGE ( 'NONE', *, *, #10330, .T. ) ;
#7677 = EDGE_LOOP ( 'NONE', ( #3956, #13646 ) ) ;
#7678 = ORIENTED_EDGE ( 'NONE', *, *, #3893, .F. ) ;
#7679 = ORIENTED_EDGE ( 'NONE', *, *, #544, .T. ) ;
#7680 = CARTESIAN_POINT ( 'NONE',  ( 116.7775623211734342, 75.03908161011133870, 0.7500000000000006661 ) ) ;
#7681 = DIRECTION ( 'NONE',  ( 0.000000000000000000, 1.000000000000000000, 0.000000000000000000 ) ) ;
#7682 = ORIENTED_EDGE ( 'NONE', *, *, #5883, .F. ) ;
#7683 = CARTESIAN_POINT ( 'NONE',  ( 116.7775623211734342, 85.03908161011133870, 19.25000000000000000 ) ) ;
#7684 = CARTESIAN_POINT ( 'NONE',  ( -17.20223088790494970, 26.94994329434792490, 56.11889009176745446 ) ) ;
#7685 = DIRECTION ( 'NONE',  ( 0.000000000000000000, 0.000000000000000000, -1.000000000000000000 ) ) ;
#7686 = CYLINDRICAL_SURFACE ( 'NONE', #7828, 4.250000000000000000 ) ;
#7687 = AXIS2_PLACEMENT_3D ( 'NONE', #4689, #11247, #3576 ) ;
#7688 = LINE ( 'NONE', #7840, #4700 ) ;
#7689 = VERTEX_POINT ( 'NONE', #570 ) ;
#7690 = ORIENTED_EDGE ( 'NONE', *, *, #13444, .F. ) ;
#7691 = EDGE_CURVE ( 'NONE', #5675, #11446, #12716, .T. ) ;
#7692 = ORIENTED_EDGE ( 'NONE', *, *, #9365, .F. ) ;
#7693 = ORIENTED_EDGE ( 'NONE', *, *, #1447, .F. ) ;
#7694 = ADVANCED_FACE ( 'NONE', ( #3169 ), #7384, .F. ) ;
#7695 = AXIS2_PLACEMENT_3D ( 'NONE', #13309, #8004, #12275 ) ;
#7696 = DIRECTION ( 'NONE',  ( 1.000000000000000000, 0.000000000000000000, 0.000000000000000000 ) ) ;
#7697 = ORIENTED_EDGE ( 'NONE', *, *, #2415, .F. ) ;
#7698 = CARTESIAN_POINT ( 'NONE',  ( 27.50000000000001066, 9.000000000000000000, 29.99999999999999645 ) ) ;
#7699 = DIRECTION ( 'NONE',  ( 1.000000000000000000, 0.000000000000000000, 0.000000000000000000 ) ) ;
#7700 = DIRECTION ( 'NONE',  ( 0.000000000000000000, 0.000000000000000000, -1.000000000000000000 ) ) ;
#7701 = DIRECTION ( 'NONE',  ( -0.9496839325805416232, -0.3132098788326400096, 0.000000000000000000 ) ) ;
#7702 = DIRECTION ( 'NONE',  ( -1.000000000000000000, -1.239088197126292296E-16, -0.000000000000000000 ) ) ;
#7703 = CARTESIAN_POINT ( 'NONE',  ( -35.72201093190194854, 10.97290950744599947, 7.250000000000000000 ) ) ;
#7704 = FACE_OUTER_BOUND ( 'NONE', #13201, .T. ) ;
#7705 = LINE ( 'NONE', #3412, #6936 ) ;
#7706 = CYLINDRICAL_SURFACE ( 'NONE', #215, 2.700000000000001066 ) ;
#7707 = AXIS2_PLACEMENT_3D ( 'NONE', #7595, #1324, #11882 ) ;
#7708 = ORIENTED_EDGE ( 'NONE', *, *, #13635, .F. ) ;
#7709 = EDGE_CURVE ( 'NONE', #11194, #8213, #5296, .T. ) ;
#7710 = ORIENTED_EDGE ( 'NONE', *, *, #2987, .F. ) ;
#7711 = ORIENTED_EDGE ( 'NONE', *, *, #3076, .F. ) ;
#7712 = PLANE ( 'NONE',  #582 ) ;
#7713 = DIRECTION ( 'NONE',  ( 1.000000000000000000, 0.000000000000000000, 0.000000000000000000 ) ) ;
#7714 = ORIENTED_EDGE ( 'NONE', *, *, #4589, .T. ) ;
#7715 = VERTEX_POINT ( 'NONE', #13805 ) ;
#7716 = DIRECTION ( 'NONE',  ( -0.000000000000000000, -0.000000000000000000, -1.000000000000000000 ) ) ;
#7717 = EDGE_LOOP ( 'NONE', ( #11198, #11106 ) ) ;
#7718 =( GEOMETRIC_REPRESENTATION_CONTEXT ( 3 ) GLOBAL_UNCERTAINTY_ASSIGNED_CONTEXT ( ( #13396 ) ) GLOBAL_UNIT_ASSIGNED_CONTEXT ( ( #4550, #7737, #4345 ) ) REPRESENTATION_CONTEXT ( 'NONE', 'WORKASPACE' ) );
#7719 = EDGE_CURVE ( 'NONE', #10426, #8976, #2825, .T. ) ;
#7720 = DIRECTION ( 'NONE',  ( 0.000000000000000000, 0.000000000000000000, 1.000000000000000000 ) ) ;
#7721 = CARTESIAN_POINT ( 'NONE',  ( -16.04064420431702942, 0.000000000000000000, -7.307586582922258600 ) ) ;
#7722 = DIRECTION ( 'NONE',  ( -1.000000000000000000, 7.097562450402079698E-15, 0.000000000000000000 ) ) ;
#7723 = CARTESIAN_POINT ( 'NONE',  ( -0.04028432657539302714, 0.000000000000000000, 16.54539866546730309 ) ) ;
#7724 = DIRECTION ( 'NONE',  ( -0.2148617826751194892, -2.631297944121794810E-17, -0.9766444667050899753 ) ) ;
#7725 = EDGE_CURVE ( 'NONE', #9665, #217, #4342, .T. ) ;
#7726 = CARTESIAN_POINT ( 'NONE',  ( -30.48673169511680214, 10.97290950744599947, 5.250000000000000000 ) ) ;
#7727 = EDGE_CURVE ( 'NONE', #9462, #6784, #3925, .T. ) ;
#7728 = CARTESIAN_POINT ( 'NONE',  ( 16.04064420431708982, 4.500000000000000000, 7.307586582922145801 ) ) ;
#7729 = VECTOR ( 'NONE', #6592, 1000.000000000000000 ) ;
#7730 = VECTOR ( 'NONE', #5358, 1000.000000000000114 ) ;
#7731 = VERTEX_POINT ( 'NONE', #12218 ) ;
#7732 = ADVANCED_FACE ( 'NONE', ( #11107 ), #1669, .T. ) ;
#7733 = EDGE_LOOP ( 'NONE', ( #8889, #8385 ) ) ;
#7734 = CARTESIAN_POINT ( 'NONE',  ( -35.05918829505000645, 10.97290950744599947, 62.14999999999999858 ) ) ;
#7735 = VERTEX_POINT ( 'NONE', #7734 ) ;
#7736 = VERTEX_POINT ( 'NONE', #551 ) ;
#7737 =( NAMED_UNIT ( * ) PLANE_ANGLE_UNIT ( ) SI_UNIT ( $, .RADIAN. ) );
#7738 = DIRECTION ( 'NONE',  ( 1.000000000000000000, 0.000000000000000000, -0.000000000000000000 ) ) ;
#7739 = CIRCLE ( 'NONE', #3090, 1.999999999999991340 ) ;
#7740 = CARTESIAN_POINT ( 'NONE',  ( 0.000000000000000000, 8.500000000000000000, 0.000000000000000000 ) ) ;
#7741 = AXIS2_PLACEMENT_3D ( 'NONE', #3273, #7482, #6468 ) ;
#7742 = DIRECTION ( 'NONE',  ( 0.000000000000000000, 0.000000000000000000, -1.000000000000000000 ) ) ;
#7743 = EDGE_CURVE ( 'NONE', #1109, #12176, #9693, .T. ) ;
#7744 = CYLINDRICAL_SURFACE ( 'NONE', #11596, 16.66282263685194920 ) ;
#7745 = CARTESIAN_POINT ( 'NONE',  ( 16.08092853089229024, 0.000000000000000000, -7.237812082545202585 ) ) ;
#7746 = AXIS2_PLACEMENT_3D ( 'NONE', #10933, #1541, #9016 ) ;
#7747 = AXIS2_PLACEMENT_3D ( 'NONE', #2459, #4742, #9917 ) ;
#7748 = CIRCLE ( 'NONE', #4430, 16.72262947720610171 ) ;
#7749 = VERTEX_POINT ( 'NONE', #13125 ) ;
#7750 = ORIENTED_EDGE ( 'NONE', *, *, #5596, .F. ) ;
#7751 = ADVANCED_FACE ( 'NONE', ( #13058 ), #12156, .F. ) ;
#7752 = CONICAL_SURFACE ( 'NONE', #8657, 8.300000000000000711, 0.08573846772804097349 ) ;
#7753 = VERTEX_POINT ( 'NONE', #5854 ) ;
#7754 = DIRECTION ( 'NONE',  ( -0.000000000000000000, 1.000000000000000000, -0.000000000000000000 ) ) ;
#7755 = ADVANCED_FACE ( 'NONE', ( #6771 ), #3703, .F. ) ;
#7756 = EDGE_LOOP ( 'NONE', ( #13142, #13642 ) ) ;
#7757 = VERTEX_POINT ( 'NONE', #3645 ) ;
#7758 = EDGE_LOOP ( 'NONE', ( #11072, #12542 ) ) ;
#7759 = CARTESIAN_POINT ( 'NONE',  ( -19.55918829504999934, 28.64232754551664684, 57.35000000000000142 ) ) ;
#7760 = CARTESIAN_POINT ( 'NONE',  ( 16.04064420431708982, 0.000000000000000000, 9.307586582922137808 ) ) ;
#7761 = VERTEX_POINT ( 'NONE', #493 ) ;
#7762 = ADVANCED_FACE ( 'NONE', ( #1459 ), #2605, .T. ) ;
#7763 = CARTESIAN_POINT ( 'NONE',  ( 44.63563590245420443, 103.9054980190242361, 22.75000000000000000 ) ) ;
#7764 = CARTESIAN_POINT ( 'NONE',  ( -17.08318469166218989, 26.94349457154494232, 56.20301699921735405 ) ) ;
#7765 = AXIS2_PLACEMENT_3D ( 'NONE', #11333, #1840, #1767 ) ;
#7766 = CIRCLE ( 'NONE', #10020, 7.166108729582679970 ) ;
#7767 = CARTESIAN_POINT ( 'NONE',  ( -19.55918829504999934, 27.40458623260099813, 57.35000000000000142 ) ) ;
#7768 = CIRCLE ( 'NONE', #4665, 24.03999999999999915 ) ;
#7769 = CARTESIAN_POINT ( 'NONE',  ( 100.2760581142613603, 115.9375248198690826, 10.00000000000000000 ) ) ;
#7770 = DIRECTION ( 'NONE',  ( 0.000000000000000000, 0.000000000000000000, 1.000000000000000000 ) ) ;
#7771 = VERTEX_POINT ( 'NONE', #10068 ) ;
#7772 = VECTOR ( 'NONE', #2475, 1000.000000000000000 ) ;
#7773 = AXIS2_PLACEMENT_3D ( 'NONE', #12192, #1497, #9045 ) ;
#7774 = CARTESIAN_POINT ( 'NONE',  ( 4.599650328638321461, 8.500000000000000000, 9.878124499050780827 ) ) ;
#7775 = ORIENTED_EDGE ( 'NONE', *, *, #10615, .T. ) ;
#7776 = DIRECTION ( 'NONE',  ( 1.000000000000000000, 0.000000000000000000, 0.000000000000000000 ) ) ;
#7777 = CARTESIAN_POINT ( 'NONE',  ( -21.51338012790479226, 30.10205818035979419, 55.47564455151579210 ) ) ;
#7778 = DIRECTION ( 'NONE',  ( 1.000000000000000000, 0.000000000000000000, 0.000000000000000000 ) ) ;
#7779 = ORIENTED_EDGE ( 'NONE', *, *, #5578, .F. ) ;
#7780 = CARTESIAN_POINT ( 'NONE',  ( -21.79515398487389888, 3.617295300293844829, 60.04999999999999716 ) ) ;
#7781 = LINE ( 'NONE', #3681, #10253 ) ;
#7782 = CARTESIAN_POINT ( 'NONE',  ( 185.2712718049083946, 108.6554980190242503, 23.00000000000000000 ) ) ;
#7783 = DIRECTION ( 'NONE',  ( -1.000000000000000000, 1.075797504481739195E-15, 0.000000000000000000 ) ) ;
#7784 = ADVANCED_FACE ( 'NONE', ( #6904 ), #12085, .F. ) ;
#7785 = AXIS2_PLACEMENT_3D ( 'NONE', #13228, #9033, #3728 ) ;
#7786 = CIRCLE ( 'NONE', #10044, 10.74999999999999645 ) ;
#7787 = CYLINDRICAL_SURFACE ( 'NONE', #5918, 1.999999999999991340 ) ;
#7788 = CARTESIAN_POINT ( 'NONE',  ( 98.63563590245422574, 99.03908161011133870, 20.00000000000000000 ) ) ;
#7789 = CARTESIAN_POINT ( 'NONE',  ( -9.759188295050000406, 10.97290950744599947, 61.86500000000000199 ) ) ;
#7790 = VERTEX_POINT ( 'NONE', #4754 ) ;
#7791 = PLANE ( 'NONE',  #3751 ) ;
#7792 = LINE ( 'NONE', #10189, #2048 ) ;
#7793 = VECTOR ( 'NONE', #10911, 1000.000000000000000 ) ;
#7794 = AXIS2_PLACEMENT_3D ( 'NONE', #1275, #8688, #10023 ) ;
#7795 = DIRECTION ( 'NONE',  ( -0.000000000000000000, -0.000000000000000000, 1.000000000000000000 ) ) ;
#7796 = DIRECTION ( 'NONE',  ( 0.000000000000000000, 0.000000000000000000, -1.000000000000000000 ) ) ;
#7797 = DIRECTION ( 'NONE',  ( 0.000000000000000000, 0.000000000000000000, 1.000000000000000000 ) ) ;
#7798 = DIRECTION ( 'NONE',  ( 0.000000000000000000, 3.387121092260455192E-15, 1.000000000000000000 ) ) ;
#7799 = CARTESIAN_POINT ( 'NONE',  ( -18.05918829504999934, 10.97290950744599947, 63.54999999999999716 ) ) ;
#7800 = DIRECTION ( 'NONE',  ( 0.000000000000000000, 0.000000000000000000, -1.000000000000000000 ) ) ;
#7801 = ADVANCED_FACE ( 'NONE', ( #9011 ), #6969, .T. ) ;
#7802 = ADVANCED_FACE ( 'NONE', ( #9991, #8022 ), #12301, .T. ) ;
#7803 = TOROIDAL_SURFACE ( 'NONE', #6476, 10.75000000000000000, 0.7500000000000000000 ) ;
#7804 = VECTOR ( 'NONE', #12841, 1000.000000000000114 ) ;
#7805 = VECTOR ( 'NONE', #10498, 1000.000000000000000 ) ;
#7806 = AXIS2_PLACEMENT_3D ( 'NONE', #6081, #4008, #9176 ) ;
#7807 = VERTEX_POINT ( 'NONE', #8800 ) ;
#7808 = DIRECTION ( 'NONE',  ( 0.000000000000000000, 0.000000000000000000, 1.000000000000000000 ) ) ;
#7809 = ORIENTED_EDGE ( 'NONE', *, *, #10046, .T. ) ;
#7810 = CARTESIAN_POINT ( 'NONE',  ( 3.940811704950003325, 32.97290950744599769, 0.000000000000000000 ) ) ;
#7811 = DIRECTION ( 'NONE',  ( 0.000000000000000000, 0.000000000000000000, 1.000000000000000000 ) ) ;
#7812 = CARTESIAN_POINT ( 'NONE',  ( 44.88563590245420443, 108.6554980190242503, 23.00000000000000000 ) ) ;
#7813 = DIRECTION ( 'NONE',  ( -1.000000000000000000, 0.000000000000000000, 0.000000000000000000 ) ) ;
#7814 = AXIS2_PLACEMENT_3D ( 'NONE', #8419, #3268, #11768 ) ;
#7815 = CIRCLE ( 'NONE', #9392, 13.50000000000000000 ) ;
#7816 = CIRCLE ( 'NONE', #3166, 6.450000000000019718 ) ;
#7817 = DIRECTION ( 'NONE',  ( 1.000000000000000000, 0.000000000000000000, 0.000000000000000000 ) ) ;
#7818 = ADVANCED_FACE ( 'NONE', ( #5646 ), #11282, .F. ) ;
#7819 = CARTESIAN_POINT ( 'NONE',  ( 44.63563590245420443, 89.90549801902423610, 23.00000000000000000 ) ) ;
#7820 = EDGE_CURVE ( 'NONE', #12394, #7171, #8945, .T. ) ;
#7821 = VERTEX_POINT ( 'NONE', #5712 ) ;
#7822 = EDGE_CURVE ( 'NONE', #1952, #7434, #416, .T. ) ;
#7823 = CIRCLE ( 'NONE', #12967, 13.50000000000000000 ) ;
#7824 = ORIENTED_EDGE ( 'NONE', *, *, #6290, .F. ) ;
#7825 = EDGE_CURVE ( 'NONE', #5985, #6783, #4808, .T. ) ;
#7826 = CARTESIAN_POINT ( 'NONE',  ( -16.52469481223740644, 30.30953598072262167, 61.33979638101006060 ) ) ;
#7827 = VECTOR ( 'NONE', #13519, 1000.000000000000000 ) ;
#7828 = AXIS2_PLACEMENT_3D ( 'NONE', #8474, #2213, #9601 ) ;
#7829 = ORIENTED_EDGE ( 'NONE', *, *, #10744, .T. ) ;
#7830 = EDGE_LOOP ( 'NONE', ( #2053, #13619, #9943, #8129 ) ) ;
#7831 = VERTEX_POINT ( 'NONE', #1820 ) ;
#7832 = ORIENTED_EDGE ( 'NONE', *, *, #9388, .T. ) ;
#7833 = DIRECTION ( 'NONE',  ( 0.000000000000000000, 0.000000000000000000, 1.000000000000000000 ) ) ;
#7834 = CARTESIAN_POINT ( 'NONE',  ( -7.241070169793070832, 29.81324547859995278, 5.250000000000000000 ) ) ;
#7835 = EDGE_LOOP ( 'NONE', ( #1121, #3926 ) ) ;
#7836 = CARTESIAN_POINT ( 'NONE',  ( -14.42040990200814043, 6.848677238728379635, 30.59999999999999787 ) ) ;
#7837 = CARTESIAN_POINT ( 'NONE',  ( -18.05918829504999934, 10.97290950744599947, 56.84999999999999432 ) ) ;
#7838 = CARTESIAN_POINT ( 'NONE',  ( -19.51818023821623882, 27.03346355975680737, 56.97665238683753586 ) ) ;
#7839 = EDGE_CURVE ( 'NONE', #5283, #6, #5459, .T. ) ;
#7840 = CARTESIAN_POINT ( 'NONE',  ( -40.05918829504999934, -14.02709049255400053, 10.00000000000000000 ) ) ;
#7841 = CIRCLE ( 'NONE', #11210, 1.999999999999991340 ) ;
#7842 = ORIENTED_EDGE ( 'NONE', *, *, #2274, .F. ) ;
#7843 = EDGE_CURVE ( 'NONE', #9433, #5595, #2037, .T. ) ;
#7844 = VERTEX_POINT ( 'NONE', #4058 ) ;
#7845 = ORIENTED_EDGE ( 'NONE', *, *, #5887, .T. ) ;
#7846 = AXIS2_PLACEMENT_3D ( 'NONE', #3963, #11299, #1805 ) ;
#7847 = FACE_OUTER_BOUND ( 'NONE', #996, .T. ) ;
#7848 = EDGE_LOOP ( 'NONE', ( #11911, #9020, #8120, #10652 ) ) ;
#7849 = DIRECTION ( 'NONE',  ( -0.3202092937642124215, -0.6304490528084107925, -0.7071067811865487940 ) ) ;
#7850 = CARTESIAN_POINT ( 'NONE',  ( -21.86795241036432813, 30.04605120275055796, 57.88020891191813888 ) ) ;
#7851 = LINE ( 'NONE', #2511, #5321 ) ;
#7852 = DIRECTION ( 'NONE',  ( 0.000000000000000000, 0.000000000000000000, 1.000000000000000000 ) ) ;
#7853 = CYLINDRICAL_SURFACE ( 'NONE', #9862, 13.50000000000000000 ) ;
#7854 = DIRECTION ( 'NONE',  ( 0.000000000000000000, 0.000000000000000000, 1.000000000000000000 ) ) ;
#7855 = SHAPE_REPRESENTATION_RELATIONSHIP ( 'NONE' , 'NONE' ,  #10413, #5740 ) ;
#7856 = ORIENTED_EDGE ( 'NONE', *, *, #3636, .T. ) ;
#7857 = VECTOR ( 'NONE', #2995, 1000.000000000000000 ) ;
#7858 = EDGE_CURVE ( 'NONE', #11822, #7715, #8304, .T. ) ;
#7859 = ORIENTED_EDGE ( 'NONE', *, *, #13245, .T. ) ;
#7860 = CARTESIAN_POINT ( 'NONE',  ( -16.20671929495594910, 8.873300352462479168, 23.90000000000000213 ) ) ;
#7861 = APPLICATION_CONTEXT ( 'automotive_design' ) ;
#7862 = DIRECTION ( 'NONE',  ( 1.000000000000000000, 0.000000000000000000, 0.000000000000000000 ) ) ;
#7863 = DIRECTION ( 'NONE',  ( -0.000000000000000000, 1.000000000000000000, -0.000000000000000000 ) ) ;
#7864 = CARTESIAN_POINT ( 'NONE',  ( 44.76431555889458735, 112.7284214383315089, 20.00000000000000000 ) ) ;
#7865 = DIRECTION ( 'NONE',  ( 0.000000000000000000, 0.000000000000000000, 1.000000000000000000 ) ) ;
#7866 = AXIS2_PLACEMENT_3D ( 'NONE', #1317, #3287, #2395 ) ;
#7867 = LINE ( 'NONE', #1591, #2722 ) ;
#7868 = DIRECTION ( 'NONE',  ( 0.6615960714621574867, -0.7498604124941119498, 0.000000000000000000 ) ) ;
#7869 = CARTESIAN_POINT ( 'NONE',  ( -16.08092853089235774, 0.000000000000000000, 7.237812082545092451 ) ) ;
#7870 = CARTESIAN_POINT ( 'NONE',  ( 44.88563590245420443, 94.90549801902425031, 22.75000000000000000 ) ) ;
#7871 = CARTESIAN_POINT ( 'NONE',  ( 140.6356359024541973, 108.9054980190242503, 22.75000000000000000 ) ) ;
#7872 = DIRECTION ( 'NONE',  ( -1.000000000000000000, 0.000000000000000000, 0.000000000000000000 ) ) ;
#7873 = CARTESIAN_POINT ( 'NONE',  ( 8.814269998155230823, -15.06602133594279991, 7.000000000000000000 ) ) ;
#7874 = CIRCLE ( 'NONE', #4234, 24.04163056034261459 ) ;
#7875 = ORIENTED_EDGE ( 'NONE', *, *, #1500, .T. ) ;
#7876 = ORIENTED_EDGE ( 'NONE', *, *, #2235, .F. ) ;
#7877 = VERTEX_POINT ( 'NONE', #12364 ) ;
#7878 = CARTESIAN_POINT ( 'NONE',  ( -39.30918829504999934, -6.027090492554000534, 64.85000000000000853 ) ) ;
#7879 = EDGE_CURVE ( 'NONE', #8989, #3167, #2811, .T. ) ;
#7880 = EDGE_CURVE ( 'NONE', #13705, #1, #5022, .T. ) ;
#7881 = ORIENTED_EDGE ( 'NONE', *, *, #9962, .F. ) ;
#7882 = ORIENTED_EDGE ( 'NONE', *, *, #2795, .T. ) ;
#7883 = CARTESIAN_POINT ( 'NONE',  ( -16.55918829504999579, 27.40458623260099813, 57.35000000000000142 ) ) ;
#7884 = DIRECTION ( 'NONE',  ( 1.000000000000000000, 0.000000000000000000, 0.000000000000000000 ) ) ;
#7885 = DIRECTION ( 'NONE',  ( 0.000000000000000000, 0.000000000000000000, 1.000000000000000000 ) ) ;
#7886 = VERTEX_POINT ( 'NONE', #818 ) ;
#7887 = ADVANCED_FACE ( 'NONE', ( #7035 ), #10172, .T. ) ;
#7888 = FACE_OUTER_BOUND ( 'NONE', #10286, .T. ) ;
#7889 = LINE ( 'NONE', #8877, #10055 ) ;
#7890 = PRODUCT_DEFINITION ( 'UNKNOWN', '', #5987, #9217 ) ;
#7891 = CARTESIAN_POINT ( 'NONE',  ( -39.30918829504999934, -6.027090492554000534, 64.35000000000000853 ) ) ;
#7892 = ORIENTED_EDGE ( 'NONE', *, *, #11434, .T. ) ;
#7893 = ORIENTED_EDGE ( 'NONE', *, *, #2548, .F. ) ;
#7894 = CARTESIAN_POINT ( 'NONE',  ( -18.05918829504999934, 30.36027202460864771, 61.70913974837019822 ) ) ;
#7895 = EDGE_LOOP ( 'NONE', ( #491, #6724, #1601, #569 ) ) ;
#7896 = ADVANCED_FACE ( 'NONE', ( #11379 ), #13472, .F. ) ;
#7897 = ORIENTED_EDGE ( 'NONE', *, *, #1091, .T. ) ;
#7898 = ADVANCED_BREP_SHAPE_REPRESENTATION ( '', ( #4512, #6434 ), #2686 ) ;
#7899 = DIRECTION ( 'NONE',  ( 0.000000000000000000, -1.000000000000000000, 0.000000000000000000 ) ) ;
#7900 = CARTESIAN_POINT ( 'NONE',  ( -1.059188295049996231, 27.97290950744599769, 58.85000000000000142 ) ) ;
#7901 = ORIENTED_EDGE ( 'NONE', *, *, #3997, .F. ) ;
#7902 = EDGE_CURVE ( 'NONE', #12702, #4150, #8909, .T. ) ;
#7903 = FACE_OUTER_BOUND ( 'NONE', #4932, .T. ) ;
#7904 = DIRECTION ( 'NONE',  ( 0.000000000000000000, 0.000000000000000000, -1.000000000000000000 ) ) ;
#7905 = CARTESIAN_POINT ( 'NONE',  ( -18.05918829504999934, 10.97290950744599947, 60.04999999999999716 ) ) ;
#7906 = DIRECTION ( 'NONE',  ( 1.000000000000000000, 0.000000000000000000, 0.000000000000000000 ) ) ;
#7907 = EDGE_CURVE ( 'NONE', #8675, #13218, #10395, .T. ) ;
#7908 = AXIS2_PLACEMENT_3D ( 'NONE', #12856, #1125, #4559 ) ;
#7909 = VERTEX_POINT ( 'NONE', #11513 ) ;
#7910 = ORIENTED_EDGE ( 'NONE', *, *, #13216, .F. ) ;
#7911 = ORIENTED_EDGE ( 'NONE', *, *, #6323, .T. ) ;
#7912 = EDGE_CURVE ( 'NONE', #10620, #12198, #5083, .T. ) ;
#7913 = CARTESIAN_POINT ( 'NONE',  ( -41.50918829505000218, 27.97290950744599769, 83.57661607529820458 ) ) ;
#7914 = DIRECTION ( 'NONE',  ( 0.000000000000000000, 0.000000000000000000, 1.000000000000000000 ) ) ;
#7915 = CIRCLE ( 'NONE', #1912, 4.749999999999997335 ) ;
#7916 = CARTESIAN_POINT ( 'NONE',  ( -21.22921039045582958, 30.14298388890195568, 54.91443165197912180 ) ) ;
#7917 = CARTESIAN_POINT ( 'NONE',  ( -6.000000000000000888, 11.99999999999999822, 7.000000000000000000 ) ) ;
#7918 = FACE_OUTER_BOUND ( 'NONE', #874, .T. ) ;
#7919 = CARTESIAN_POINT ( 'NONE',  ( -9.562604962050000879, 19.46949284044600148, 60.04999999999999716 ) ) ;
#7920 = EDGE_CURVE ( 'NONE', #13003, #2432, #10272, .T. ) ;
#7921 = CARTESIAN_POINT ( 'NONE',  ( -21.05918829504999934, 10.97290950744599947, 116.8499999999999943 ) ) ;
#7922 = PRODUCT_DEFINITION_SHAPE ( 'NONE', 'NONE',  #13812 ) ;
#7923 = DIRECTION ( 'NONE',  ( 0.000000000000000000, 0.000000000000000000, 1.000000000000000000 ) ) ;
#7924 = ORIENTED_EDGE ( 'NONE', *, *, #10739, .F. ) ;
#7925 = AXIS2_PLACEMENT_3D ( 'NONE', #534, #9051, #7927 ) ;
#7926 = EDGE_CURVE ( 'NONE', #6706, #4329, #5243, .T. ) ;
#7927 = DIRECTION ( 'NONE',  ( 1.000000000000000000, 0.000000000000000000, 0.000000000000000000 ) ) ;
#7928 = DIRECTION ( 'NONE',  ( 0.000000000000000000, 0.000000000000000000, 1.000000000000000000 ) ) ;
#7929 = VERTEX_POINT ( 'NONE', #6191 ) ;
#7930 = CARTESIAN_POINT ( 'NONE',  ( -22.58763155544259860, 2.057013498776719906, 62.85000000000000142 ) ) ;
#7931 = LINE ( 'NONE', #1589, #9314 ) ;
#7932 = ADVANCED_FACE ( 'NONE', ( #3082 ), #4956, .T. ) ;
#7933 = FACE_OUTER_BOUND ( 'NONE', #11598, .T. ) ;
#7934 = DIRECTION ( 'NONE',  ( -0.7071067811865474617, -0.7071067811865474617, 0.000000000000000000 ) ) ;
#7935 = FACE_OUTER_BOUND ( 'NONE', #3435, .T. ) ;
#7936 = DIRECTION ( 'NONE',  ( 1.000000000000000000, 0.000000000000000000, 0.000000000000000000 ) ) ;
#7937 = LINE ( 'NONE', #2596, #1299 ) ;
#7938 = DIRECTION ( 'NONE',  ( 0.000000000000000000, 0.000000000000000000, 1.000000000000000000 ) ) ;
#7939 = AXIS2_PLACEMENT_3D ( 'NONE', #13363, #10412, #3098 ) ;
#7940 = EDGE_CURVE ( 'NONE', #11264, #1821, #7030, .T. ) ;
#7941 = DIRECTION ( 'NONE',  ( 0.000000000000000000, 1.000000000000000000, 0.000000000000000000 ) ) ;
#7942 = CARTESIAN_POINT ( 'NONE',  ( 44.76431555889458735, 112.7284214383315089, 3.521624574640407997E-16 ) ) ;
#7943 = UNCERTAINTY_MEASURE_WITH_UNIT (LENGTH_MEASURE( 1.000000000000000082E-05 ), #9239, 'distance_accuracy_value', 'NONE');
#7944 = VERTEX_POINT ( 'NONE', #3912 ) ;
#7945 = VECTOR ( 'NONE', #10205, 1000.000000000000000 ) ;
#7946 = DIRECTION ( 'NONE',  ( -1.000000000000000000, 0.000000000000000000, 0.000000000000000000 ) ) ;
#7947 = VERTEX_POINT ( 'NONE', #8161 ) ;
#7948 = EDGE_LOOP ( 'NONE', ( #2953, #12990, #10761, #8703 ) ) ;
#7949 = CYLINDRICAL_SURFACE ( 'NONE', #10637, 3.000000000000002665 ) ;
#7950 = LINE ( 'NONE', #6974, #5133 ) ;
#7951 = DIRECTION ( 'NONE',  ( 0.000000000000000000, 1.000000000000000000, 0.000000000000000000 ) ) ;
#7952 = DIRECTION ( 'NONE',  ( -0.000000000000000000, -0.000000000000000000, -1.000000000000000000 ) ) ;
#7953 = CARTESIAN_POINT ( 'NONE',  ( -34.21925492805003444, 2.892876190445991202, 63.34900083300006202 ) ) ;
#7954 = CYLINDRICAL_SURFACE ( 'NONE', #888, 12.00000000000000355 ) ;
#7955 = VECTOR ( 'NONE', #12352, 1000.000000000000000 ) ;
#7956 = CARTESIAN_POINT ( 'NONE',  ( -24.37001676333060018, -4.028726038184999858, 62.14999999999999858 ) ) ;
#7957 = EDGE_CURVE ( 'NONE', #12322, #10219, #6061, .T. ) ;
#7958 = ORIENTED_EDGE ( 'NONE', *, *, #730, .T. ) ;
#7959 = EDGE_LOOP ( 'NONE', ( #7204, #10467 ) ) ;
#7960 = DIRECTION ( 'NONE',  ( 0.000000000000000000, 1.000000000000000000, 0.000000000000000000 ) ) ;
#7961 = VECTOR ( 'NONE', #5474, 999.9999999999998863 ) ;
#7962 = ORIENTED_EDGE ( 'NONE', *, *, #12693, .F. ) ;
#7963 = ORIENTED_EDGE ( 'NONE', *, *, #3553, .T. ) ;
#7964 = CIRCLE ( 'NONE', #1968, 6.749999999999999112 ) ;
#7965 = DIRECTION ( 'NONE',  ( -0.000000000000000000, -0.000000000000000000, 1.000000000000000000 ) ) ;
#7966 = ORIENTED_EDGE ( 'NONE', *, *, #13296, .F. ) ;
#7967 = CARTESIAN_POINT ( 'NONE',  ( 140.6356359024541973, 94.90549801902425031, 23.00000000000000000 ) ) ;
#7968 = CARTESIAN_POINT ( 'NONE',  ( -18.05918829504999934, 3.352862570446000223, 61.63595870800000398 ) ) ;
#7969 = ORIENTED_EDGE ( 'NONE', *, *, #8517, .F. ) ;
#7970 = DIRECTION ( 'NONE',  ( 0.000000000000000000, -1.000000000000000000, 0.000000000000000000 ) ) ;
#7971 = ORIENTED_EDGE ( 'NONE', *, *, #12998, .T. ) ;
#7972 = CARTESIAN_POINT ( 'NONE',  ( -18.05918829505001000, 19.19006679501500656, 63.35000000030875356 ) ) ;
#7973 = CARTESIAN_POINT ( 'NONE',  ( -5.809188295050001116, -6.027090492554000534, 7.250000000000000000 ) ) ;
#7974 = DIRECTION ( 'NONE',  ( 0.000000000000000000, 0.000000000000000000, -1.000000000000000000 ) ) ;
#7975 = ADVANCED_FACE ( 'NONE', ( #2102 ), #3278, .T. ) ;
#7976 = DIRECTION ( 'NONE',  ( -1.000000000000000000, 0.000000000000000000, 0.000000000000000000 ) ) ;
#7977 = AXIS2_PLACEMENT_3D ( 'NONE', #4026, #7148, #7074 ) ;
#7978 = ORIENTED_EDGE ( 'NONE', *, *, #4766, .T. ) ;
#7979 = VECTOR ( 'NONE', #2281, 1000.000000000000000 ) ;
#7980 = EDGE_CURVE ( 'NONE', #11868, #4563, #12893, .T. ) ;
#7981 = VECTOR ( 'NONE', #2785, 1000.000000000000000 ) ;
#7982 = ORIENTED_EDGE ( 'NONE', *, *, #12434, .T. ) ;
#7983 = DIRECTION ( 'NONE',  ( 1.000000000000000000, 0.000000000000000000, 0.000000000000000000 ) ) ;
#7984 = EDGE_CURVE ( 'NONE', #11929, #6593, #11319, .T. ) ;
#7985 = ORIENTED_EDGE ( 'NONE', *, *, #2617, .F. ) ;
#7986 = CIRCLE ( 'NONE', #1522, 8.250000000000001776 ) ;
#7987 = CIRCLE ( 'NONE', #3984, 24.92993838181874722 ) ;
#7988 = AXIS2_PLACEMENT_3D ( 'NONE', #2818, #13410, #4066 ) ;
#7989 = AXIS2_PLACEMENT_3D ( 'NONE', #9308, #709, #9244 ) ;
#7990 = CARTESIAN_POINT ( 'NONE',  ( -21.37927600327723354, 30.12180271171412826, 59.51279792984109207 ) ) ;
#7991 = ORIENTED_EDGE ( 'NONE', *, *, #5201, .T. ) ;
#7992 = CARTESIAN_POINT ( 'NONE',  ( 185.2712718049083946, 0.000000000000000000, 23.00000000000000000 ) ) ;
#7993 = CARTESIAN_POINT ( 'NONE',  ( 81.82136590429890077, 114.1051029460540605, 10.00000000000000000 ) ) ;
#7994 = CARTESIAN_POINT ( 'NONE',  ( -8.499999999999998224, 2.000000000000000000, -65.00000000000000000 ) ) ;
#7995 = DIRECTION ( 'NONE',  ( 3.614007241618347908E-17, -1.000000000000000000, 0.000000000000000000 ) ) ;
#7996 = FACE_BOUND ( 'NONE', #2695, .T. ) ;
#7997 = CARTESIAN_POINT ( 'NONE',  ( 0.000000000000000000, 0.000000000000000000, 64.85000000000000853 ) ) ;
#7998 = EDGE_CURVE ( 'NONE', #5796, #12702, #2237, .T. ) ;
#7999 = AXIS2_PLACEMENT_3D ( 'NONE', #889, #3016, #8223 ) ;
#8000 = CIRCLE ( 'NONE', #11134, 6.145833333000000565 ) ;
#8001 = CIRCLE ( 'NONE', #4223, 2.000000000000001776 ) ;
#8002 = VECTOR ( 'NONE', #2804, 1000.000000000000000 ) ;
#8003 = EDGE_CURVE ( 'NONE', #9556, #722, #10832, .T. ) ;
#8004 = DIRECTION ( 'NONE',  ( 0.000000000000000000, 0.000000000000000000, -1.000000000000000000 ) ) ;
#8005 = DIRECTION ( 'NONE',  ( 0.000000000000000000, 0.000000000000000000, -1.000000000000000000 ) ) ;
#8006 = ORIENTED_EDGE ( 'NONE', *, *, #7691, .T. ) ;
#8007 = CARTESIAN_POINT ( 'NONE',  ( -18.05918829504999934, 10.97290950744599947, 60.40999999999999659 ) ) ;
#8008 = DIRECTION ( 'NONE',  ( 0.000000000000000000, 0.000000000000000000, 1.000000000000000000 ) ) ;
#8009 = DIRECTION ( 'NONE',  ( 1.000000000000000000, 3.614007241618347908E-17, 0.000000000000000000 ) ) ;
#8010 = ADVANCED_FACE ( 'NONE', ( #2808 ), #8153, .F. ) ;
#8011 = CARTESIAN_POINT ( 'NONE',  ( -22.66538754097585340, 13.57680303481476614, 68.55875404394534200 ) ) ;
#8012 = CYLINDRICAL_SURFACE ( 'NONE', #2006, 2.999999999999998224 ) ;
#8013 = CARTESIAN_POINT ( 'NONE',  ( 140.3249757306743675, 112.2890816101113387, 0.000000000000000000 ) ) ;
#8014 = FACE_OUTER_BOUND ( 'NONE', #2241, .T. ) ;
#8015 = CARTESIAN_POINT ( 'NONE',  ( 142.6356359024541973, 111.0390816101113103, 0.3106601717798236351 ) ) ;
#8016 = AXIS2_PLACEMENT_3D ( 'NONE', #13633, #2911, #4143 ) ;
#8017 = CARTESIAN_POINT ( 'NONE',  ( -18.05918829504999934, 10.97290950744599947, 62.14999999999999858 ) ) ;
#8018 = EDGE_CURVE ( 'NONE', #1491, #3000, #12701, .T. ) ;
#8019 = ORIENTED_EDGE ( 'NONE', *, *, #4248, .F. ) ;
#8020 = EDGE_CURVE ( 'NONE', #1848, #1852, #3149, .T. ) ;
#8021 = AXIS2_PLACEMENT_3D ( 'NONE', #11185, #4697, #1613 ) ;
#8022 = FACE_OUTER_BOUND ( 'NONE', #12127, .T. ) ;
#8023 = AXIS2_PLACEMENT_3D ( 'NONE', #12133, #2648, #9963 ) ;
#8024 = EDGE_LOOP ( 'NONE', ( #12844, #7414, #1335, #7054 ) ) ;
#8025 = VERTEX_POINT ( 'NONE', #1229 ) ;
#8026 = DIRECTION ( 'NONE',  ( -0.000000000000000000, -0.000000000000000000, 1.000000000000000000 ) ) ;
#8027 = CARTESIAN_POINT ( 'NONE',  ( -38.38077571930826082, 22.44393519180575680, 17.25000000000000000 ) ) ;
#8028 = CARTESIAN_POINT ( 'NONE',  ( -18.05918829504999934, 10.97290950744599947, 67.84999999999999432 ) ) ;
#8029 = FACE_OUTER_BOUND ( 'NONE', #7630, .T. ) ;
#8030 = CARTESIAN_POINT ( 'NONE',  ( -35.05918829505000645, -6.027090492554000534, 17.25000000000000000 ) ) ;
#8031 = DIRECTION ( 'NONE',  ( 1.000000000000000000, 0.000000000000000000, 0.000000000000000000 ) ) ;
#8032 = CARTESIAN_POINT ( 'NONE',  ( 12.81426999815521839, -15.06602133594279991, 0.000000000000000000 ) ) ;
#8033 = CIRCLE ( 'NONE', #4040, 15.45000000000000462 ) ;
#8034 = VECTOR ( 'NONE', #8438, 1000.000000000000000 ) ;
#8035 = CIRCLE ( 'NONE', #12714, 4.750000000000000000 ) ;
#8036 = ORIENTED_EDGE ( 'NONE', *, *, #2614, .F. ) ;
#8037 = FACE_OUTER_BOUND ( 'NONE', #6422, .T. ) ;
#8038 = ORIENTED_EDGE ( 'NONE', *, *, #12475, .F. ) ;
#8039 = CARTESIAN_POINT ( 'NONE',  ( -20.70557258089865016, 13.97235115742243927, 30.59999999999999787 ) ) ;
#8040 = ORIENTED_EDGE ( 'NONE', *, *, #13308, .F. ) ;
#8041 = AXIS2_PLACEMENT_3D ( 'NONE', #4802, #13111, #5970 ) ;
#8042 = AXIS2_PLACEMENT_3D ( 'NONE', #1256, #10772, #6633 ) ;
#8043 = FACE_BOUND ( 'NONE', #8887, .T. ) ;
#8044 = AXIS2_PLACEMENT_3D ( 'NONE', #13728, #8221, #8362 ) ;
#8045 = CARTESIAN_POINT ( 'NONE',  ( -18.05918829504999934, 18.13068114044600065, 61.70038048199999281 ) ) ;
#8046 = ADVANCED_FACE ( 'NONE', ( #10603, #11928, #6547, #10747, #5421, #3219, #8434, #10814 ), #5481, .F. ) ;
#8047 = DIRECTION ( 'NONE',  ( -0.000000000000000000, -0.000000000000000000, -1.000000000000000000 ) ) ;
#8048 = VERTEX_POINT ( 'NONE', #1028 ) ;
#8049 = CARTESIAN_POINT ( 'NONE',  ( 7.347880794884120722E-16, -17.50000000000000000, -6.000000000000000888 ) ) ;
#8050 = DIRECTION ( 'NONE',  ( 0.000000000000000000, 0.000000000000000000, 1.000000000000000000 ) ) ;
#8051 = DIRECTION ( 'NONE',  ( 1.000000000000000000, 0.000000000000000000, 0.000000000000000000 ) ) ;
#8052 = CARTESIAN_POINT ( 'NONE',  ( -35.05918829505000645, 27.97290950744599769, 64.85000000000000853 ) ) ;
#8053 = AXIS2_PLACEMENT_3D ( 'NONE', #3505, #12090, #5650 ) ;
#8054 = AXIS2_PLACEMENT_3D ( 'NONE', #10787, #1064, #3390 ) ;
#8055 = APPLICATION_CONTEXT ( 'automotive_design' ) ;
#8056 = VECTOR ( 'NONE', #3210, 1000.000000000000114 ) ;
#8057 = VERTEX_POINT ( 'NONE', #1095 ) ;
#8058 = ORIENTED_EDGE ( 'NONE', *, *, #11732, .T. ) ;
#8059 = ORIENTED_EDGE ( 'NONE', *, *, #4200, .T. ) ;
#8060 = ORIENTED_EDGE ( 'NONE', *, *, #5245, .T. ) ;
#8061 = EDGE_CURVE ( 'NONE', #6439, #12897, #12771, .T. ) ;
#8062 = ORIENTED_EDGE ( 'NONE', *, *, #4200, .F. ) ;
#8063 = EDGE_CURVE ( 'NONE', #5932, #939, #7370, .T. ) ;
#8064 = CARTESIAN_POINT ( 'NONE',  ( -25.29804148384604900, -2.574630058508220021, 62.14999999999999858 ) ) ;
#8065 = EDGE_LOOP ( 'NONE', ( #11396, #13038, #1378, #10043, #11584 ) ) ;
#8066 = CARTESIAN_POINT ( 'NONE',  ( -20.84781795900099155, 30.19228463275523566, 60.32764583509811018 ) ) ;
#8067 = AXIS2_PLACEMENT_3D ( 'NONE', #10753, #10610, #1171 ) ;
#8068 = AXIS2_PLACEMENT_3D ( 'NONE', #2425, #13151, #12177 ) ;
#8069 = CARTESIAN_POINT ( 'NONE',  ( -18.05918829504999934, 10.97290950744599947, 63.14999999999999858 ) ) ;
#8070 = AXIS2_PLACEMENT_3D ( 'NONE', #8759, #4368, #6525 ) ;
#8071 = DIRECTION ( 'NONE',  ( 1.000000000000000000, 0.000000000000000000, -0.000000000000000000 ) ) ;
#8072 = FACE_OUTER_BOUND ( 'NONE', #4205, .T. ) ;
#8073 = DIRECTION ( 'NONE',  ( 1.000000000000000000, 0.000000000000000000, 0.000000000000000000 ) ) ;
#8074 = DIRECTION ( 'NONE',  ( 0.000000000000000000, 0.000000000000000000, 1.000000000000000000 ) ) ;
#8075 = EDGE_LOOP ( 'NONE', ( #13702, #7676 ) ) ;
#8076 = VECTOR ( 'NONE', #10262, 1000.000000000000114 ) ;
#8077 = DIRECTION ( 'NONE',  ( 1.000000000000000000, 0.000000000000000000, 0.000000000000000000 ) ) ;
#8078 = ORIENTED_EDGE ( 'NONE', *, *, #7081, .F. ) ;
#8079 = EDGE_LOOP ( 'NONE', ( #7551, #10625, #7875, #6864 ) ) ;
#8080 = CARTESIAN_POINT ( 'NONE',  ( -34.72201093190195564, 10.97290950744599947, 5.250000000000000000 ) ) ;
#8081 = EDGE_CURVE ( 'NONE', #9242, #3266, #13734, .T. ) ;
#8082 = DIRECTION ( 'NONE',  ( 0.000000000000000000, 0.000000000000000000, 1.000000000000000000 ) ) ;
#8083 = FACE_OUTER_BOUND ( 'NONE', #1670, .T. ) ;
#8084 = DIRECTION ( 'NONE',  ( 1.000000000000000000, 0.000000000000000000, 0.000000000000000000 ) ) ;
#8085 = DIRECTION ( 'NONE',  ( -0.7071067811865451302, 0.7071067811865500152, -0.000000000000000000 ) ) ;
#8086 = DIRECTION ( 'NONE',  ( 0.4678190685372686231, -0.5302313826179265721, 0.7071067811865505703 ) ) ;
#8087 = EDGE_CURVE ( 'NONE', #12491, #10270, #12826, .T. ) ;
#8088 = DIRECTION ( 'NONE',  ( 0.000000000000000000, 0.000000000000000000, 1.000000000000000000 ) ) ;
#8089 = LINE ( 'NONE', #11163, #5354 ) ;
#8090 = CIRCLE ( 'NONE', #3425, 16.75000000000000355 ) ;
#8091 = CARTESIAN_POINT ( 'NONE',  ( 42.63563590245419732, 113.0390816101113387, 20.00000000000000000 ) ) ;
#8092 = LINE ( 'NONE', #752, #192 ) ;
#8093 = EDGE_CURVE ( 'NONE', #8866, #12554, #6608, .T. ) ;
#8094 = UNCERTAINTY_MEASURE_WITH_UNIT (LENGTH_MEASURE( 1.000000000000000082E-05 ), #538, 'distance_accuracy_value', 'NONE');
#8095 =( BOUNDED_CURVE ( )  B_SPLINE_CURVE ( 3, ( #1632, #5882, #1697, #5942 ),
 .UNSPECIFIED., .F., .F. ) 
 B_SPLINE_CURVE_WITH_KNOTS ( ( 4, 4 ),
 ( 1.570796326794896558, 3.141592653589793116 ),
 .UNSPECIFIED. ) 
 CURVE ( )  GEOMETRIC_REPRESENTATION_ITEM ( )  RATIONAL_B_SPLINE_CURVE ( ( 1.000000000000000000, 0.8047378541243649375, 0.8047378541243649375, 1.000000000000000000 ) ) 
 REPRESENTATION_ITEM ( '' )  );
#8096 = ORIENTED_EDGE ( 'NONE', *, *, #12274, .F. ) ;
#8097 = ORIENTED_EDGE ( 'NONE', *, *, #5599, .F. ) ;
#8098 = CARTESIAN_POINT ( 'NONE',  ( 42.63563590245419732, 87.03908161011136713, 20.00000000000000000 ) ) ;
#8099 = ORIENTED_EDGE ( 'NONE', *, *, #3948, .T. ) ;
#8100 = ORIENTED_EDGE ( 'NONE', *, *, #3063, .T. ) ;
#8102 = EDGE_CURVE ( 'NONE', #3976, #12622, #10376, .T. ) ;
#8101 = ORIENTED_EDGE ( 'NONE', *, *, #4075, .F. ) ;
#8103 = FACE_OUTER_BOUND ( 'NONE', #8974, .T. ) ;
#8104 = DIRECTION ( 'NONE',  ( 0.000000000000000000, -1.000000000000000000, 0.000000000000000000 ) ) ;
#8105 = CARTESIAN_POINT ( 'NONE',  ( 8.814269998155230823, -15.06602133594279991, 0.000000000000000000 ) ) ;
#8106 = EDGE_CURVE ( 'NONE', #4562, #10360, #7915, .T. ) ;
#8107 = FACE_OUTER_BOUND ( 'NONE', #12509, .T. ) ;
#8108 = CYLINDRICAL_SURFACE ( 'NONE', #11149, 4.250000000000000000 ) ;
#8109 = EDGE_CURVE ( 'NONE', #68, #5925, #9715, .T. ) ;
#8110 = CARTESIAN_POINT ( 'NONE',  ( 44.63563590245420443, 94.90549801902425031, 22.75000000000000000 ) ) ;
#8111 = VECTOR ( 'NONE', #2285, 1000.000000000000000 ) ;
#8112 = ORIENTED_EDGE ( 'NONE', *, *, #9078, .T. ) ;
#8113 = ORIENTED_EDGE ( 'NONE', *, *, #11055, .F. ) ;
#8114 = CARTESIAN_POINT ( 'NONE',  ( -15.86143927199362302, 30.25607652234101863, 60.91235729977573499 ) ) ;
#8115 = ORIENTED_EDGE ( 'NONE', *, *, #10330, .F. ) ;
#8116 = ORIENTED_EDGE ( 'NONE', *, *, #9831, .T. ) ;
#8117 = DIRECTION ( 'NONE',  ( 0.000000000000000000, 0.000000000000000000, -1.000000000000000000 ) ) ;
#8118 = FACE_OUTER_BOUND ( 'NONE', #11867, .T. ) ;
#8119 = VERTEX_POINT ( 'NONE', #4796 ) ;
#8120 = ORIENTED_EDGE ( 'NONE', *, *, #6802, .F. ) ;
#8121 = CARTESIAN_POINT ( 'NONE',  ( 50.63563590245420443, 94.90549801902425031, 23.00000000000000000 ) ) ;
#8122 = CYLINDRICAL_SURFACE ( 'NONE', #6438, 1.999999999999991340 ) ;
#8123 = PLANE ( 'NONE',  #7806 ) ;
#8124 = DIRECTION ( 'NONE',  ( 1.000000000000000000, 0.000000000000000000, 0.000000000000000000 ) ) ;
#8125 = CYLINDRICAL_SURFACE ( 'NONE', #6898, 4.749999999999997335 ) ;
#8126 = EDGE_CURVE ( 'NONE', #1567, #2972, #4668, .T. ) ;
#8127 = CYLINDRICAL_SURFACE ( 'NONE', #9393, 2.700000000000001066 ) ;
#8128 = ORIENTED_EDGE ( 'NONE', *, *, #3997, .T. ) ;
#8129 = ORIENTED_EDGE ( 'NONE', *, *, #1897, .F. ) ;
#8130 = LINE ( 'NONE', #7207, #2672 ) ;
#8131 = CARTESIAN_POINT ( 'NONE',  ( -19.87176177124059251, 30.28946906204819101, 61.18505942812437581 ) ) ;
#8132 = CARTESIAN_POINT ( 'NONE',  ( 116.7775623211734342, 75.03908161011133870, 0.000000000000000000 ) ) ;
#8133 = CARTESIAN_POINT ( 'NONE',  ( -8.499999999999998224, 2.000000000000000000, -65.00000000000000000 ) ) ;
#8134 = DIRECTION ( 'NONE',  ( -0.000000000000000000, -0.000000000000000000, 1.000000000000000000 ) ) ;
#8135 = CARTESIAN_POINT ( 'NONE',  ( 92.63563590245421153, 99.03908161011133870, 20.00000000000000000 ) ) ;
#8136 = APPLICATION_PROTOCOL_DEFINITION ( 'draft international standard', 'automotive_design', 1998, #9568 ) ;
#8137 = APPLICATION_CONTEXT ( 'automotive_design' ) ;
#8138 = EDGE_LOOP ( 'NONE', ( #9728, #1682, #5172, #12894 ) ) ;
#8139 = EDGE_CURVE ( 'NONE', #9940, #13024, #8922, .T. ) ;
#8140 = EDGE_CURVE ( 'NONE', #12773, #803, #6590, .T. ) ;
#8141 = AXIS2_PLACEMENT_3D ( 'NONE', #5924, #5998, #11259 ) ;
#8142 = DIRECTION ( 'NONE',  ( 0.000000000000000000, 0.000000000000000000, -1.000000000000000000 ) ) ;
#8143 = ORIENTED_EDGE ( 'NONE', *, *, #1679, .T. ) ;
#8144 = CARTESIAN_POINT ( 'NONE',  ( -7.999999999999998224, 2.000000000000000000, -65.00000000000000000 ) ) ;
#8145 = CARTESIAN_POINT ( 'NONE',  ( -16.04064420431702942, 4.500000000000000000, -9.307586582922249718 ) ) ;
#8146 = FACE_OUTER_BOUND ( 'NONE', #3084, .T. ) ;
#8147 = CARTESIAN_POINT ( 'NONE',  ( -4.599650328638321461, 8.500000000000001776, -7.878124499050794149 ) ) ;
#8148 = ORIENTED_EDGE ( 'NONE', *, *, #1439, .F. ) ;
#8149 = FACE_OUTER_BOUND ( 'NONE', #11431, .T. ) ;
#8150 = FACE_OUTER_BOUND ( 'NONE', #8601, .T. ) ;
#8151 = CARTESIAN_POINT ( 'NONE',  ( 4.599650328638321461, 8.500000000000000000, 7.878124499050794149 ) ) ;
#8152 = DIRECTION ( 'NONE',  ( 0.000000000000000000, 0.000000000000000000, 1.000000000000000000 ) ) ;
#8153 = CYLINDRICAL_SURFACE ( 'NONE', #1297, 2.000000000000001776 ) ;
#8154 = AXIS2_PLACEMENT_3D ( 'NONE', #12240, #4831, #2696 ) ;
#8155 = VECTOR ( 'NONE', #6477, 1000.000000000000227 ) ;
#8156 = EDGE_CURVE ( 'NONE', #13231, #3610, #2163, .T. ) ;
#8157 = EDGE_CURVE ( 'NONE', #4997, #6, #270, .T. ) ;
#8158 = VERTEX_POINT ( 'NONE', #9973 ) ;
#8159 = EDGE_CURVE ( 'NONE', #2432, #10425, #1442, .T. ) ;
#8160 = ORIENTED_EDGE ( 'NONE', *, *, #10346, .T. ) ;
#8161 = CARTESIAN_POINT ( 'NONE',  ( -4.059188295049996675, 27.97290950744599769, 0.000000000000000000 ) ) ;
#8162 = VERTEX_POINT ( 'NONE', #3753 ) ;
#8163 = CARTESIAN_POINT ( 'NONE',  ( -21.09568578533284011, 14.96173881432403086, 68.84049927876318975 ) ) ;
#8164 = PRODUCT_RELATED_PRODUCT_CATEGORY ( 'part', '', ( #3300 ) ) ;
#8165 = CIRCLE ( 'NONE', #12837, 23.29163056034261459 ) ;
#8166 = FACE_OUTER_BOUND ( 'NONE', #5644, .T. ) ;
#8167 = EDGE_CURVE ( 'NONE', #3998, #11468, #8992, .T. ) ;
#8168 = CARTESIAN_POINT ( 'NONE',  ( 43.38563590245419732, 110.7284214383315089, 0.000000000000000000 ) ) ;
#8169 = DIRECTION ( 'NONE',  ( -1.000000000000000000, 0.000000000000000000, -0.000000000000000000 ) ) ;
#8170 = CARTESIAN_POINT ( 'NONE',  ( 50.63563590245420443, 90.15549801902423610, 22.75000000000000000 ) ) ;
#8171 = DIRECTION ( 'NONE',  ( 0.4528443260392608916, 0.8915896008669279560, 0.000000000000000000 ) ) ;
#8172 = ADVANCED_FACE ( 'NONE', ( #11091 ), #8784, .F. ) ;
#8173 = ORIENTED_EDGE ( 'NONE', *, *, #3970, .T. ) ;
#8174 = CARTESIAN_POINT ( 'NONE',  ( -14.86617432291880370, 30.13979931665073408, 59.74664482119747078 ) ) ;
#8175 = ORIENTED_EDGE ( 'NONE', *, *, #11671, .F. ) ;
#8176 = ADVANCED_FACE ( 'NONE', ( #9849 ), #7712, .T. ) ;
#8177 = FILL_AREA_STYLE_COLOUR ( '', #3027 ) ;
#8178 = CARTESIAN_POINT ( 'NONE',  ( -16.07440008066354764, 8.723328269963658954, 27.09999999999999787 ) ) ;
#8179 = ORIENTED_EDGE ( 'NONE', *, *, #3860, .T. ) ;
#8180 = DIRECTION ( 'NONE',  ( -0.7091883091770476710, -0.7050191076322684935, 0.000000000000000000 ) ) ;
#8181 = CARTESIAN_POINT ( 'NONE',  ( 142.6356359024541973, 87.03908161011133870, 0.3106601717798216367 ) ) ;
#8182 = EDGE_LOOP ( 'NONE', ( #220, #9104 ) ) ;
#8183 = AXIS2_PLACEMENT_3D ( 'NONE', #1399, #3705, #496 ) ;
#8184 = CARTESIAN_POINT ( 'NONE',  ( -11.70083760351054103, 35.47811937223634970, 17.25000000000000000 ) ) ;
#8185 = DIRECTION ( 'NONE',  ( 0.000000000000000000, 0.000000000000000000, 1.000000000000000000 ) ) ;
#8186 = CARTESIAN_POINT ( 'NONE',  ( -19.26019363180991206, 27.93101569915827653, 58.27028413769223647 ) ) ;
#8187 = DIRECTION ( 'NONE',  ( 0.7071067811865505703, 0.000000000000000000, 0.7071067811865444641 ) ) ;
#8188 = EDGE_CURVE ( 'NONE', #9150, #9852, #11956, .T. ) ;
#8189 = VECTOR ( 'NONE', #8289, 1000.000000000000000 ) ;
#8190 = CIRCLE ( 'NONE', #7066, 1.999999999999991340 ) ;
#8191 = VERTEX_POINT ( 'NONE', #2454 ) ;
#8192 = ORIENTED_EDGE ( 'NONE', *, *, #6328, .F. ) ;
#8193 = EDGE_LOOP ( 'NONE', ( #7859, #11196, #9634, #7678 ) ) ;
#8194 = EDGE_CURVE ( 'NONE', #2353, #5798, #5703, .T. ) ;
#8195 = PLANE ( 'NONE',  #6639 ) ;
#8196 = CARTESIAN_POINT ( 'NONE',  ( -19.10156701222420850, 30.33693478205813676, 61.54316241360875495 ) ) ;
#8197 = AXIS2_PLACEMENT_3D ( 'NONE', #11831, #13651, #8546 ) ;
#8198 = CYLINDRICAL_SURFACE ( 'NONE', #1853, 6.145833333000002341 ) ;
#8199 = VECTOR ( 'NONE', #12353, 1000.000000000000000 ) ;
#8200 = LINE ( 'NONE', #6163, #3528 ) ;
#8201 = DIRECTION ( 'NONE',  ( 1.000000000000000000, 0.000000000000000000, 0.000000000000000000 ) ) ;
#8202 = CIRCLE ( 'NONE', #8421, 0.5000000000000000000 ) ;
#8203 = PLANE ( 'NONE',  #2480 ) ;
#8204 = CARTESIAN_POINT ( 'NONE',  ( -47.05918829505009882, 8.972909507444612132, 157.8500000000000512 ) ) ;
#8205 = VERTEX_POINT ( 'NONE', #12201 ) ;
#8206 = VERTEX_POINT ( 'NONE', #333 ) ;
#8207 = CIRCLE ( 'NONE', #3095, 6.449999999999997513 ) ;
#8208 = AXIS2_PLACEMENT_3D ( 'NONE', #9054, #4152, #5249 ) ;
#8209 = VECTOR ( 'NONE', #13611, 1000.000000000000000 ) ;
#8210 = CIRCLE ( 'NONE', #9555, 8.300000000000000711 ) ;
#8211 = CARTESIAN_POINT ( 'NONE',  ( 140.5069562460138286, 112.7284214383315089, 4.059660689008197386E-16 ) ) ;
#8212 = DIRECTION ( 'NONE',  ( 0.000000000000000000, 0.000000000000000000, 1.000000000000000000 ) ) ;
#8213 = VERTEX_POINT ( 'NONE', #6681 ) ;
#8214 = FACE_OUTER_BOUND ( 'NONE', #13605, .T. ) ;
#8215 = CARTESIAN_POINT ( 'NONE',  ( -8.500289910546818817, -3.085093966544980137, 62.14999999999999858 ) ) ;
#8216 = CARTESIAN_POINT ( 'NONE',  ( -18.05918829504999934, 10.97290950744599947, 57.35000000000000142 ) ) ;
#8217 = DIRECTION ( 'NONE',  ( 0.000000000000000000, 0.000000000000000000, 1.000000000000000000 ) ) ;
#8218 = CARTESIAN_POINT ( 'NONE',  ( 68.49370948373500312, 112.2890816101113387, 20.00000000000000000 ) ) ;
#8219 = DIRECTION ( 'NONE',  ( 1.000000000000000000, 0.000000000000000000, 0.000000000000000000 ) ) ;
#8220 = EDGE_CURVE ( 'NONE', #4278, #7243, #4605, .T. ) ;
#8221 = DIRECTION ( 'NONE',  ( 0.000000000000000000, 0.000000000000000000, 1.000000000000000000 ) ) ;
#8222 = CARTESIAN_POINT ( 'NONE',  ( 140.3856359024541973, 108.6554980190242503, 23.00000000000000000 ) ) ;
#8223 = DIRECTION ( 'NONE',  ( 1.000000000000000000, 0.000000000000000000, 0.000000000000000000 ) ) ;
#8224 = VECTOR ( 'NONE', #485, 1000.000000000000000 ) ;
#8225 = VERTEX_POINT ( 'NONE', #2727 ) ;
#8226 = AXIS2_PLACEMENT_3D ( 'NONE', #13147, #11267, #1691 ) ;
#8227 = AXIS2_PLACEMENT_3D ( 'NONE', #10809, #7426, #1221 ) ;
#8228 = CIRCLE ( 'NONE', #180, 18.00000000000000000 ) ;
#8229 = ORIENTED_EDGE ( 'NONE', *, *, #8478, .T. ) ;
#8230 = CARTESIAN_POINT ( 'NONE',  ( -18.05918829504999934, 10.97290950744599947, 58.35000000000000142 ) ) ;
#8231 = ORIENTED_EDGE ( 'NONE', *, *, #13794, .T. ) ;
#8232 = AXIS2_PLACEMENT_3D ( 'NONE', #10115, #2013, #12548 ) ;
#8233 = ORIENTED_EDGE ( 'NONE', *, *, #11878, .T. ) ;
#8234 = ORIENTED_EDGE ( 'NONE', *, *, #10585, .T. ) ;
#8235 = CARTESIAN_POINT ( 'NONE',  ( 84.99521369064696330, 82.14063840035363739, 20.00000000000000000 ) ) ;
#8236 = AXIS2_PLACEMENT_3D ( 'NONE', #3410, #10874, #1294 ) ;
#8237 = CARTESIAN_POINT ( 'NONE',  ( -39.80918829504999934, 27.97290950744599769, 68.85549045786049760 ) ) ;
#8238 = CARTESIAN_POINT ( 'NONE',  ( 116.7775623211734342, 75.03908161011133870, 19.25000000000000000 ) ) ;
#8239 = CARTESIAN_POINT ( 'NONE',  ( -18.05918829504999934, 10.00028003023991907, 62.14999999999999858 ) ) ;
#8240 = CIRCLE ( 'NONE', #7544, 2.000000000000001776 ) ;
#8241 = ADVANCED_FACE ( 'NONE', ( #1303 ), #10885, .T. ) ;
#8242 = DIRECTION ( 'NONE',  ( 0.000000000000000000, 1.000000000000000000, 0.000000000000000000 ) ) ;
#8243 = DIRECTION ( 'NONE',  ( 1.000000000000000000, 0.000000000000000000, -0.000000000000000000 ) ) ;
#8244 = CIRCLE ( 'NONE', #4902, 20.00000000000000000 ) ;
#8245 = AXIS2_PLACEMENT_3D ( 'NONE', #12965, #12765, #12889 ) ;
#8246 = ORIENTED_EDGE ( 'NONE', *, *, #2449, .F. ) ;
#8247 = CARTESIAN_POINT ( 'NONE',  ( -15.15614148912509229, 30.17819129753064544, 54.51704934337099218 ) ) ;
#8248 = ORIENTED_EDGE ( 'NONE', *, *, #9722, .F. ) ;
#8249 = ORIENTED_EDGE ( 'NONE', *, *, #504, .T. ) ;
#8250 = DIRECTION ( 'NONE',  ( 0.000000000000000000, 0.000000000000000000, -1.000000000000000000 ) ) ;
#8251 = LINE ( 'NONE', #12723, #9914 ) ;
#8252 = DIRECTION ( 'NONE',  ( 0.000000000000000000, -1.000000000000000000, 0.000000000000000000 ) ) ;
#8253 = ORIENTED_EDGE ( 'NONE', *, *, #5080, .F. ) ;
#8254 = CARTESIAN_POINT ( 'NONE',  ( -18.05918829504999934, 10.97290950744599947, 61.10999999999999943 ) ) ;
#8255 = CARTESIAN_POINT ( 'NONE',  ( -14.32322260522609980, 18.32852371459815188, 60.04999999999999716 ) ) ;
#8256 = EDGE_CURVE ( 'NONE', #651, #912, #5631, .T. ) ;
#8257 = ORIENTED_EDGE ( 'NONE', *, *, #1310, .F. ) ;
#8258 = DIRECTION ( 'NONE',  ( 1.000000000000000000, 0.000000000000000000, 0.000000000000000000 ) ) ;
#8259 = AXIS2_PLACEMENT_3D ( 'NONE', #3653, #13207, #5652 ) ;
#8260 = CARTESIAN_POINT ( 'NONE',  ( 44.88563590245420443, 94.65549801902425031, 23.00000000000000000 ) ) ;
#8261 = AXIS2_PLACEMENT_3D ( 'NONE', #2429, #5669, #7623 ) ;
#8262 = ADVANCED_FACE ( 'NONE', ( #13104 ), #7787, .F. ) ;
#8263 = CARTESIAN_POINT ( 'NONE',  ( -38.63164489498320364, 10.97290950744599947, 7.250000000000000000 ) ) ;
#8264 = DIRECTION ( 'NONE',  ( 0.000000000000000000, -1.000000000000000000, 0.000000000000000000 ) ) ;
#8265 = EDGE_CURVE ( 'NONE', #11879, #12380, #347, .T. ) ;
#8266 = VECTOR ( 'NONE', #4534, 1000.000000000000000 ) ;
#8267 = AXIS2_PLACEMENT_3D ( 'NONE', #12330, #6087, #12453 ) ;
#8268 = CIRCLE ( 'NONE', #2039, 6.850000000000002309 ) ;
#8269 = ORIENTED_EDGE ( 'NONE', *, *, #12712, .T. ) ;
#8270 = ORIENTED_EDGE ( 'NONE', *, *, #1051, .F. ) ;
#8271 = ORIENTED_EDGE ( 'NONE', *, *, #5655, .T. ) ;
#8272 = CARTESIAN_POINT ( 'NONE',  ( -2.059188295050000228, 10.97290950744599947, 56.84999999999999432 ) ) ;
#8273 = ADVANCED_FACE ( 'NONE', ( #5692 ), #600, .F. ) ;
#8274 = FACE_OUTER_BOUND ( 'NONE', #8883, .T. ) ;
#8275 = CARTESIAN_POINT ( 'NONE',  ( -9.861988295050000630, 2.775709507445999868, 63.35000000000000142 ) ) ;
#8276 = DIRECTION ( 'NONE',  ( 0.000000000000000000, 1.000000000000000000, 0.000000000000000000 ) ) ;
#8277 = CYLINDRICAL_SURFACE ( 'NONE', #10983, 4.750000000000000888 ) ;
#8278 = CARTESIAN_POINT ( 'NONE',  ( 44.63563590245420443, 89.90549801902423610, 20.00000000000000000 ) ) ;
#8279 = AXIS2_PLACEMENT_3D ( 'NONE', #4516, #6668, #7699 ) ;
#8280 = VECTOR ( 'NONE', #12429, 1000.000000000000000 ) ;
#8281 = CARTESIAN_POINT ( 'NONE',  ( -18.05918829505000289, 10.97290950744599414, 105.8500000000000085 ) ) ;
#8282 = VERTEX_POINT ( 'NONE', #6105 ) ;
#8283 = CIRCLE ( 'NONE', #5815, 6.450000000000001066 ) ;
#8284 = VERTEX_POINT ( 'NONE', #10183 ) ;
#8285 = EDGE_CURVE ( 'NONE', #6318, #11722, #11509, .T. ) ;
#8286 = PRESENTATION_LAYER_ASSIGNMENT (  '', '', ( #7156 ) ) ;
#8287 = DIRECTION ( 'NONE',  ( 0.000000000000000000, 0.000000000000000000, -1.000000000000000000 ) ) ;
#8288 = CIRCLE ( 'NONE', #3617, 4.000000000000000888 ) ;
#8289 = DIRECTION ( 'NONE',  ( -0.000000000000000000, -0.000000000000000000, -1.000000000000000000 ) ) ;
#8290 = AXIS2_PLACEMENT_3D ( 'NONE', #6243, #9325, #13578 ) ;
#8291 = EDGE_LOOP ( 'NONE', ( #735, #97, #1408, #8192 ) ) ;
#8292 = DIRECTION ( 'NONE',  ( 0.4528443260392610026, 0.8915896008669278450, 0.000000000000000000 ) ) ;
#8293 = CARTESIAN_POINT ( 'NONE',  ( -30.30918829504999934, 27.97290950744599769, 64.85000000000000853 ) ) ;
#8294 = CARTESIAN_POINT ( 'NONE',  ( -18.05918829504999934, 10.97290950744599947, 62.14999999999999858 ) ) ;
#8295 = DIRECTION ( 'NONE',  ( 0.000000000000000000, 0.000000000000000000, 1.000000000000000000 ) ) ;
#8296 = CARTESIAN_POINT ( 'NONE',  ( 68.49370948373500312, 75.03908161011133870, 19.25000000000000000 ) ) ;
#8297 = DIRECTION ( 'NONE',  ( 0.000000000000000000, 0.000000000000000000, 1.000000000000000000 ) ) ;
#8298 = DIRECTION ( 'NONE',  ( 0.000000000000000000, 0.000000000000000000, -1.000000000000000000 ) ) ;
#8299 = DIRECTION ( 'NONE',  ( 0.000000000000000000, 0.000000000000000000, 1.000000000000000000 ) ) ;
#8300 = FACE_BOUND ( 'NONE', #3667, .T. ) ;
#8301 = EDGE_CURVE ( 'NONE', #4997, #12239, #5028, .T. ) ;
#8302 = VERTEX_POINT ( 'NONE', #5135 ) ;
#8303 = VERTEX_POINT ( 'NONE', #4034 ) ;
#8304 = LINE ( 'NONE', #8098, #786 ) ;
#8305 = ORIENTED_EDGE ( 'NONE', *, *, #7619, .T. ) ;
#8306 = ORIENTED_EDGE ( 'NONE', *, *, #12611, .F. ) ;
#8307 = CARTESIAN_POINT ( 'NONE',  ( 7.640422211807137209, 16.89844320975774750, -3.000000000000000000 ) ) ;
#8308 = AXIS2_PLACEMENT_3D ( 'NONE', #7223, #9339, #6179 ) ;
#8309 = LINE ( 'NONE', #9436, #6035 ) ;
#8310 =( LENGTH_UNIT ( ) NAMED_UNIT ( * ) SI_UNIT ( .MILLI., .METRE. ) );
#8311 = LINE ( 'NONE', #13479, #12015 ) ;
#8312 = LINE ( 'NONE', #7310, #5512 ) ;
#8313 = EDGE_CURVE ( 'NONE', #4612, #10749, #5465, .T. ) ;
#8314 = ADVANCED_FACE ( 'NONE', ( #3957 ), #5964, .F. ) ;
#8315 = ORIENTED_EDGE ( 'NONE', *, *, #1897, .T. ) ;
#8316 = EDGE_CURVE ( 'NONE', #1491, #10398, #9333, .T. ) ;
#8317 = CARTESIAN_POINT ( 'NONE',  ( -15.08247214573220241, 30.16892808493238221, 60.08567788817938293 ) ) ;
#8318 = VERTEX_POINT ( 'NONE', #9127 ) ;
#8319 = EDGE_CURVE ( 'NONE', #9069, #13237, #11429, .T. ) ;
#8320 = ORIENTED_EDGE ( 'NONE', *, *, #9599, .F. ) ;
#8321 = EDGE_LOOP ( 'NONE', ( #12170, #6037, #2688, #5317 ) ) ;
#8322 = DIRECTION ( 'NONE',  ( 1.000000000000000000, 0.000000000000000000, 0.000000000000000000 ) ) ;
#8323 = APPLICATION_CONTEXT ( 'automotive_design' ) ;
#8324 = CYLINDRICAL_SURFACE ( 'NONE', #1354, 2.700000000000000178 ) ;
#8325 = ORIENTED_EDGE ( 'NONE', *, *, #7907, .T. ) ;
#8326 = CARTESIAN_POINT ( 'NONE',  ( -14.75120793773922045, 7.223607444975439940, 68.84999999999999432 ) ) ;
#8327 = DIRECTION ( 'NONE',  ( 1.000000000000000000, -0.000000000000000000, -0.000000000000000000 ) ) ;
#8328 = ORIENTED_EDGE ( 'NONE', *, *, #2235, .T. ) ;
#8329 = DIRECTION ( 'NONE',  ( 1.000000000000000000, 0.000000000000000000, 0.000000000000000000 ) ) ;
#8330 = AXIS2_PLACEMENT_3D ( 'NONE', #7130, #6015, #4979 ) ;
#8331 = CYLINDRICAL_SURFACE ( 'NONE', #3655, 16.00000000000000355 ) ;
#8332 = DIRECTION ( 'NONE',  ( 1.000000000000000000, 0.000000000000000000, 0.000000000000000000 ) ) ;
#8333 = DIRECTION ( 'NONE',  ( 0.000000000000000000, 0.000000000000000000, -1.000000000000000000 ) ) ;
#8334 = ORIENTED_EDGE ( 'NONE', *, *, #9444, .T. ) ;
#8335 = EDGE_CURVE ( 'NONE', #1822, #95, #12180, .T. ) ;
#8336 = AXIS2_PLACEMENT_3D ( 'NONE', #9061, #5570, #7227 ) ;
#8337 = EDGE_LOOP ( 'NONE', ( #9448, #1336, #8128, #1193 ) ) ;
#8338 = ORIENTED_EDGE ( 'NONE', *, *, #2449, .T. ) ;
#8339 = EDGE_CURVE ( 'NONE', #5130, #11676, #8382, .T. ) ;
#8340 = ORIENTED_EDGE ( 'NONE', *, *, #11252, .F. ) ;
#8341 = VERTEX_POINT ( 'NONE', #2859 ) ;
#8342 = DIRECTION ( 'NONE',  ( -0.000000000000000000, -1.000000000000000000, -0.000000000000000000 ) ) ;
#8343 = CARTESIAN_POINT ( 'NONE',  ( -20.46575897078212947, 30.23534695989346233, 60.73312205491463089 ) ) ;
#8344 = DIRECTION ( 'NONE',  ( 0.000000000000000000, 0.000000000000000000, 1.000000000000000000 ) ) ;
#8345 = PLANE ( 'NONE',  #2651 ) ;
#8346 = DIRECTION ( 'NONE',  ( 0.000000000000000000, -1.000000000000000000, 0.000000000000000000 ) ) ;
#8347 = CARTESIAN_POINT ( 'NONE',  ( -6.000000000000000888, -12.00000000000000178, 7.000000000000000000 ) ) ;
#8348 = SHAPE_DEFINITION_REPRESENTATION ( #7497, #10413 ) ;
#8349 = ORIENTED_EDGE ( 'NONE', *, *, #13449, .F. ) ;
#8350 = EDGE_CURVE ( 'NONE', #1667, #1818, #2394, .T. ) ;
#8351 = DIRECTION ( 'NONE',  ( 0.000000000000000000, 0.000000000000000000, -1.000000000000000000 ) ) ;
#8352 = ORIENTED_EDGE ( 'NONE', *, *, #10678, .T. ) ;
#8353 = VERTEX_POINT ( 'NONE', #4935 ) ;
#8354 = DIRECTION ( 'NONE',  ( -1.000000000000000000, 0.000000000000000000, -0.000000000000000000 ) ) ;
#8355 = CARTESIAN_POINT ( 'NONE',  ( 50.63563590245420443, 89.90549801902423610, 22.75000000000000000 ) ) ;
#8356 = EDGE_CURVE ( 'NONE', #2296, #5219, #9202, .T. ) ;
#8357 = DIRECTION ( 'NONE',  ( -0.4528443260392609471, -0.8915896008669278450, 0.000000000000000000 ) ) ;
#8358 = DIRECTION ( 'NONE',  ( 0.000000000000000000, 0.000000000000000000, 1.000000000000000000 ) ) ;
#8359 = ORIENTED_EDGE ( 'NONE', *, *, #5707, .F. ) ;
#8360 = CARTESIAN_POINT ( 'NONE',  ( 44.88563590245420443, 104.1554980190242361, 23.00000000000000000 ) ) ;
#8361 = DIRECTION ( 'NONE',  ( 0.4528443260392607250, 0.8915896008669278450, 0.000000000000000000 ) ) ;
#8362 = DIRECTION ( 'NONE',  ( 1.000000000000000000, 0.000000000000000000, 0.000000000000000000 ) ) ;
#8363 = CARTESIAN_POINT ( 'NONE',  ( -36.21615338608749823, 23.36596564213564875, 7.250000000000000000 ) ) ;
#8364 =( NAMED_UNIT ( * ) PLANE_ANGLE_UNIT ( ) SI_UNIT ( $, .RADIAN. ) );
#8365 = EDGE_CURVE ( 'NONE', #6548, #10843, #11227, .T. ) ;
#8366 = EDGE_LOOP ( 'NONE', ( #9373, #13567, #4074, #9440 ) ) ;
#8367 = AXIS2_PLACEMENT_3D ( 'NONE', #7956, #2822, #9159 ) ;
#8368 = ORIENTED_EDGE ( 'NONE', *, *, #1969, .F. ) ;
#8369 = DIRECTION ( 'NONE',  ( 0.000000000000000000, 0.000000000000000000, 1.000000000000000000 ) ) ;
#8370 = VERTEX_POINT ( 'NONE', #5063 ) ;
#8371 = CLOSED_SHELL ( 'NONE', ( #8010, #8445, #1331, #12490, #8542, #205, #1314, #6460, #10030, #1616, #7732, #6088, #7311, #8563, #11991, #8314, #9948, #1504, #6627, #8273, #7348, #4271, #11154, #11343, #3196, #4433, #12801, #10406, #6588, #3262, #11260, #1732, #12269, #7975, #7470, #3778, #3992, #3573, #11817, #5558, #247, #6204, #4016, #4701, #6952, #10799, #4510, #1885, #5619, #12346, #11992, #629, #6799, #9591, #10003, #13067, #1131, #950, #6781, #465, #7282, #11793, #650, #12795, #128, #13529, #7300, #1365, #1627, #9298, #10742, #5872, #10828, #1176, #2112, #3335, #10285, #11627, #6883, #9729, #4338, #5117, #1988, #11420, #13438, #3194, #12704, #9628, #11560, #3133, #8763, #6693, #5361, #13322, #5434, #7201, #9432, #2477, #12577, #13102, #1700, #4340, #8795, #13091, #12307, #3399 ) ) ;
#8372 = ORIENTED_EDGE ( 'NONE', *, *, #2635, .F. ) ;
#8373 = CARTESIAN_POINT ( 'NONE',  ( -20.08141632792401765, 15.85662095137910299, 68.56416753914237461 ) ) ;
#8374 = EDGE_LOOP ( 'NONE', ( #6924, #4721, #6865, #717 ) ) ;
#8375 = EDGE_CURVE ( 'NONE', #4458, #2858, #1650, .T. ) ;
#8376 = CARTESIAN_POINT ( 'NONE',  ( -35.05918829505000645, 27.97290950744599769, 17.25000000000000000 ) ) ;
#8377 = DIRECTION ( 'NONE',  ( 0.000000000000000000, 0.000000000000000000, 1.000000000000000000 ) ) ;
#8378 = VECTOR ( 'NONE', #4123, 1000.000000000000000 ) ;
#8379 =( BOUNDED_CURVE ( )  B_SPLINE_CURVE ( 3, ( #13240, #3743, #2444, #5825 ),
 .UNSPECIFIED., .F., .F. ) 
 B_SPLINE_CURVE_WITH_KNOTS ( ( 4, 4 ),
 ( 0.000000000000000000, 1.570796326794896558 ),
 .UNSPECIFIED. ) 
 CURVE ( )  GEOMETRIC_REPRESENTATION_ITEM ( )  RATIONAL_B_SPLINE_CURVE ( ( 1.000000000000000000, 0.8047378541243649375, 0.8047378541243649375, 1.000000000000000000 ) ) 
 REPRESENTATION_ITEM ( '' )  );
#8380 = DIRECTION ( 'NONE',  ( 1.000000000000000000, 0.000000000000000000, 0.000000000000000000 ) ) ;
#8381 = ORIENTED_EDGE ( 'NONE', *, *, #1133, .F. ) ;
#8382 = CIRCLE ( 'NONE', #6813, 6.000000000000005329 ) ;
#8383 = CARTESIAN_POINT ( 'NONE',  ( -14.88916620013386272, 30.14298388896176917, 59.78556834882314064 ) ) ;
#8384 = VERTEX_POINT ( 'NONE', #1796 ) ;
#8385 = ORIENTED_EDGE ( 'NONE', *, *, #4696, .F. ) ;
#8386 = EDGE_LOOP ( 'NONE', ( #11416, #2417, #5786, #8270 ) ) ;
#8387 = ORIENTED_EDGE ( 'NONE', *, *, #13512, .T. ) ;
#8388 = FACE_OUTER_BOUND ( 'NONE', #7032, .T. ) ;
#8389 = CARTESIAN_POINT ( 'NONE',  ( -19.71317847370539766, 12.84756053868127879, 53.85000000000000142 ) ) ;
#8390 = LINE ( 'NONE', #13625, #11847 ) ;
#8391 = DIRECTION ( 'NONE',  ( 0.000000000000000000, 0.000000000000000000, 1.000000000000000000 ) ) ;
#8392 = DIRECTION ( 'NONE',  ( 0.000000000000000000, 0.000000000000000000, -1.000000000000000000 ) ) ;
#8393 = DIRECTION ( 'NONE',  ( -0.4528443260392611136, -0.8915896008669277339, 0.000000000000000000 ) ) ;
#8394 = CARTESIAN_POINT ( 'NONE',  ( -18.81733386491350046, 27.95698799050449423, 58.65942797322944813 ) ) ;
#8395 = EDGE_CURVE ( 'NONE', #11676, #5130, #3939, .T. ) ;
#8396 = AXIS2_PLACEMENT_3D ( 'NONE', #2403, #12840, #4280 ) ;
#8397 = FACE_OUTER_BOUND ( 'NONE', #1186, .T. ) ;
#8398 = VERTEX_POINT ( 'NONE', #2796 ) ;
#8399 = ORIENTED_EDGE ( 'NONE', *, *, #2164, .F. ) ;
#8400 = ORIENTED_EDGE ( 'NONE', *, *, #4090, .F. ) ;
#8401 = CONICAL_SURFACE ( 'NONE', #5719, 6.419999999999999929, 0.2165503049760889864 ) ;
#8402 = CARTESIAN_POINT ( 'NONE',  ( 92.63563590245421153, 112.2890816101113387, 0.000000000000000000 ) ) ;
#8403 = DIRECTION ( 'NONE',  ( -0.000000000000000000, -0.000000000000000000, -1.000000000000000000 ) ) ;
#8404 = ORIENTED_EDGE ( 'NONE', *, *, #2869, .T. ) ;
#8405 = CARTESIAN_POINT ( 'NONE',  ( -18.62921962108772789, 26.96311099516080034, 55.95402353264894657 ) ) ;
#8406 = CARTESIAN_POINT ( 'NONE',  ( -15.05918829504999756, 10.97290950744599947, 116.8499999999999943 ) ) ;
#8407 = DIRECTION ( 'NONE',  ( 0.000000000000000000, 0.000000000000000000, 1.000000000000000000 ) ) ;
#8408 = EDGE_CURVE ( 'NONE', #11490, #13362, #740, .T. ) ;
#8409 = DIRECTION ( 'NONE',  ( 0.000000000000000000, 0.000000000000000000, -1.000000000000000000 ) ) ;
#8410 = CONTEXT_DEPENDENT_SHAPE_REPRESENTATION ( #1177, #225 ) ;
#8411 = AXIS2_PLACEMENT_3D ( 'NONE', #3004, #8212, #7218 ) ;
#8412 = PRESENTATION_LAYER_ASSIGNMENT (  '', '', ( #4629 ) ) ;
#8413 = ORIENTED_EDGE ( 'NONE', *, *, #2752, .T. ) ;
#8414 = ORIENTED_EDGE ( 'NONE', *, *, #36, .T. ) ;
#8415 = CARTESIAN_POINT ( 'NONE',  ( 111.0903281124166710, 100.8715034839261762, 10.00000000000000000 ) ) ;
#8416 = AXIS2_PLACEMENT_3D ( 'NONE', #2788, #10246, #13505 ) ;
#8417 = DIRECTION ( 'NONE',  ( 0.000000000000000000, 0.000000000000000000, 1.000000000000000000 ) ) ;
#8418 = ORIENTED_EDGE ( 'NONE', *, *, #12862, .F. ) ;
#8419 = CARTESIAN_POINT ( 'NONE',  ( 43.38563590245419732, 99.03908161011133870, 19.25000000000000000 ) ) ;
#8420 = CARTESIAN_POINT ( 'NONE',  ( 3.940811704950003325, 35.97290950744599058, 10.00000000000000000 ) ) ;
#8421 = AXIS2_PLACEMENT_3D ( 'NONE', #169, #3407, #4446 ) ;
#8422 = DIRECTION ( 'NONE',  ( -1.000000000000000000, 0.000000000000000000, 0.000000000000000000 ) ) ;
#8423 = DIRECTION ( 'NONE',  ( 0.000000000000000000, 0.000000000000000000, 1.000000000000000000 ) ) ;
#8424 = ORIENTED_EDGE ( 'NONE', *, *, #12125, .F. ) ;
#8425 = DIRECTION ( 'NONE',  ( 1.000000000000000000, 0.000000000000000000, 0.000000000000000000 ) ) ;
#8426 = LINE ( 'NONE', #5413, #7961 ) ;
#8427 = DIRECTION ( 'NONE',  ( 1.000000000000000000, 0.000000000000000000, 0.000000000000000000 ) ) ;
#8428 = EDGE_CURVE ( 'NONE', #6209, #1587, #5252, .T. ) ;
#8429 = DIRECTION ( 'NONE',  ( 0.000000000000000000, 0.000000000000000000, 1.000000000000000000 ) ) ;
#8430 = AXIS2_PLACEMENT_3D ( 'NONE', #11727, #1102, #12985 ) ;
#8431 = VECTOR ( 'NONE', #8468, 1000.000000000000000 ) ;
#8432 = VECTOR ( 'NONE', #1556, 1000.000000000000000 ) ;
#8433 = EDGE_CURVE ( 'NONE', #8341, #4986, #2085, .T. ) ;
#8434 = FACE_BOUND ( 'NONE', #12197, .T. ) ;
#8435 = VERTEX_POINT ( 'NONE', #96 ) ;
#8436 = ORIENTED_EDGE ( 'NONE', *, *, #66, .T. ) ;
#8437 = DIRECTION ( 'NONE',  ( 0.000000000000000000, 0.000000000000000000, 1.000000000000000000 ) ) ;
#8438 = DIRECTION ( 'NONE',  ( -0.3202092937642119774, -0.6304490528084089052, 0.7071067811865507924 ) ) ;
#8439 = DIRECTION ( 'NONE',  ( 0.000000000000000000, 0.000000000000000000, 1.000000000000000000 ) ) ;
#8440 = VECTOR ( 'NONE', #5844, 1000.000000000000000 ) ;
#8441 = CARTESIAN_POINT ( 'NONE',  ( 50.38563590245420443, 0.000000000000000000, 23.00000000000000000 ) ) ;
#8442 = EDGE_CURVE ( 'NONE', #7612, #9088, #2608, .T. ) ;
#8443 = VECTOR ( 'NONE', #10491, 1000.000000000000114 ) ;
#8444 = DIRECTION ( 'NONE',  ( 0.000000000000000000, -1.000000000000000000, 3.387121092260456770E-15 ) ) ;
#8445 = ADVANCED_FACE ( 'NONE', ( #8618 ), #5205, .F. ) ;
#8446 = PRODUCT_DEFINITION_FORMATION_WITH_SPECIFIED_SOURCE ( 'ANY', '', #7628, .NOT_KNOWN. ) ;
#8447 = AXIS2_PLACEMENT_3D ( 'NONE', #5213, #4451, #9483 ) ;
#8448 = EDGE_LOOP ( 'NONE', ( #10671, #5556, #4870, #13469 ) ) ;
#8449 = AXIS2_PLACEMENT_3D ( 'NONE', #5007, #12483, #10534 ) ;
#8450 = CARTESIAN_POINT ( 'NONE',  ( -14.31571447708356537, 30.05678106874812627, 56.42374946802869573 ) ) ;
#8451 = ORIENTED_EDGE ( 'NONE', *, *, #8481, .F. ) ;
#8452 = CYLINDRICAL_SURFACE ( 'NONE', #1471, 1.725000000000000755 ) ;
#8453 = CARTESIAN_POINT ( 'NONE',  ( -12.70965068984842006, 8.255843551210428899, 57.35000000000000142 ) ) ;
#8454 = CARTESIAN_POINT ( 'NONE',  ( -8.500000000000000000, 2.499999999999999556, 0.000000000000000000 ) ) ;
#8455 = LINE ( 'NONE', #13556, #1755 ) ;
#8456 = LINE ( 'NONE', #4081, #8443 ) ;
#8457 = CARTESIAN_POINT ( 'NONE',  ( -18.05918829504999223, 19.28555359244598932, 63.26601075299999621 ) ) ;
#8458 = CYLINDRICAL_SURFACE ( 'NONE', #7576, 33.00000000000000000 ) ;
#8459 = CIRCLE ( 'NONE', #6457, 2.700000000000001066 ) ;
#8460 = EDGE_CURVE ( 'NONE', #172, #8947, #11843, .T. ) ;
#8461 = ORIENTED_EDGE ( 'NONE', *, *, #2404, .T. ) ;
#8462 = VERTEX_POINT ( 'NONE', #2298 ) ;
#8463 = ORIENTED_EDGE ( 'NONE', *, *, #3698, .F. ) ;
#8464 = EDGE_CURVE ( 'NONE', #12738, #11762, #10392, .T. ) ;
#8465 = ORIENTED_EDGE ( 'NONE', *, *, #12457, .F. ) ;
#8466 = AXIS2_PLACEMENT_3D ( 'NONE', #2728, #6682, #2657 ) ;
#8467 = VECTOR ( 'NONE', #5534, 1000.000000000000000 ) ;
#8468 = DIRECTION ( 'NONE',  ( 0.000000000000000000, 0.000000000000000000, -1.000000000000000000 ) ) ;
#8469 = CARTESIAN_POINT ( 'NONE',  ( -38.05918829504999934, 10.97290950744600124, 11.50000000000000000 ) ) ;
#8470 = ORIENTED_EDGE ( 'NONE', *, *, #4901, .F. ) ;
#8471 = DIRECTION ( 'NONE',  ( 0.000000000000000000, 0.000000000000000000, -1.000000000000000000 ) ) ;
#8472 = DIRECTION ( 'NONE',  ( 1.000000000000000000, 0.000000000000000000, 0.000000000000000000 ) ) ;
#8473 = DIRECTION ( 'NONE',  ( -0.4528443260392609471, -0.8915896008669278450, 0.000000000000000000 ) ) ;
#8474 = CARTESIAN_POINT ( 'NONE',  ( -35.05918829505000645, -6.027090492554000534, 64.85000000000000853 ) ) ;
#8475 = CARTESIAN_POINT ( 'NONE',  ( 2.877919977996279531E-15, 4.500000000000000000, 23.49999999999999645 ) ) ;
#8476 = VECTOR ( 'NONE', #6758, 1000.000000000000000 ) ;
#8477 = AXIS2_PLACEMENT_3D ( 'NONE', #1400, #4617, #3293 ) ;
#8478 = EDGE_CURVE ( 'NONE', #9965, #1667, #4372, .T. ) ;
#8479 = CIRCLE ( 'NONE', #4921, 6.000000000000000888 ) ;
#8480 = VECTOR ( 'NONE', #7194, 1000.000000000000000 ) ;
#8481 = EDGE_CURVE ( 'NONE', #10025, #12322, #5405, .T. ) ;
#8482 = ORIENTED_EDGE ( 'NONE', *, *, #6770, .T. ) ;
#8483 = ADVANCED_FACE ( 'NONE', ( #165 ), #1211, .T. ) ;
#8484 = LINE ( 'NONE', #2151, #6602 ) ;
#8485 = VERTEX_POINT ( 'NONE', #12812 ) ;
#8486 = CARTESIAN_POINT ( 'NONE',  ( 44.94629607423404849, 85.78908161011133870, 0.000000000000000000 ) ) ;
#8487 = EDGE_CURVE ( 'NONE', #13343, #5535, #9609, .T. ) ;
#8488 = CARTESIAN_POINT ( 'NONE',  ( -7.241070169793063727, -7.867426463707971607, 5.250000000000000000 ) ) ;
#8489 = FILL_AREA_STYLE ('',( #7635 ) ) ;
#8490 = CARTESIAN_POINT ( 'NONE',  ( -20.17834884677884943, 30.26343021279967616, 53.72583902890555407 ) ) ;
#8491 = CIRCLE ( 'NONE', #3606, 33.00000000000000000 ) ;
#8492 = CIRCLE ( 'NONE', #4273, 0.5000000000000004441 ) ;
#8493 = CARTESIAN_POINT ( 'NONE',  ( -25.64433075620760150, -3.961216307075045240, 57.35000000000000142 ) ) ;
#8494 = DIRECTION ( 'NONE',  ( 0.000000000000000000, 0.000000000000000000, -1.000000000000000000 ) ) ;
#8495 = AXIS2_PLACEMENT_3D ( 'NONE', #6183, #10457, #8626 ) ;
#8496 = CARTESIAN_POINT ( 'NONE',  ( -38.38077571930826082, -0.4981161769137699147, 5.250000000000000000 ) ) ;
#8497 = DIRECTION ( 'NONE',  ( 0.000000000000000000, 0.000000000000000000, -1.000000000000000000 ) ) ;
#8498 = LINE ( 'NONE', #2307, #1561 ) ;
#8499 = ORIENTED_EDGE ( 'NONE', *, *, #12419, .F. ) ;
#8500 = VECTOR ( 'NONE', #3962, 1000.000000000000000 ) ;
#8501 = CIRCLE ( 'NONE', #4508, 3.000000000000002665 ) ;
#8502 = ADVANCED_FACE ( 'NONE', ( #9535 ), #6532, .F. ) ;
#8503 = ORIENTED_EDGE ( 'NONE', *, *, #12957, .F. ) ;
#8504 = CARTESIAN_POINT ( 'NONE',  ( -23.57208814848684852, -7.366404416634599883, 63.45000000000000284 ) ) ;
#8505 = ORIENTED_EDGE ( 'NONE', *, *, #3531, .T. ) ;
#8506 = ORIENTED_EDGE ( 'NONE', *, *, #9403, .F. ) ;
#8507 = ORIENTED_EDGE ( 'NONE', *, *, #414, .F. ) ;
#8508 = CARTESIAN_POINT ( 'NONE',  ( -14.75120793773922045, 7.223607444975439940, 68.84999999999999432 ) ) ;
#8509 = EDGE_CURVE ( 'NONE', #11762, #11089, #8165, .T. ) ;
#8510 = DIRECTION ( 'NONE',  ( 5.059610138265691632E-16, 1.000000000000000000, -0.000000000000000000 ) ) ;
#8511 = CARTESIAN_POINT ( 'NONE',  ( -6.000000000000000888, 7.347880794884120722E-16, 0.000000000000000000 ) ) ;
#8512 = DIRECTION ( 'NONE',  ( 0.000000000000000000, 0.000000000000000000, 1.000000000000000000 ) ) ;
#8513 = AXIS2_PLACEMENT_3D ( 'NONE', #6066, #5021, #10681 ) ;
#8514 = DIRECTION ( 'NONE',  ( 0.000000000000000000, 0.000000000000000000, 1.000000000000000000 ) ) ;
#8515 = B_SPLINE_CURVE_WITH_KNOTS ( 'NONE', 3,
 ( #12573, #12499, #8163, #11381, #1741, #3083, #12428, #975, #11516, #7176, #9434, #13678, #7301, #4126, #4190, #8373, #10338, #9358, #6127 ),
 .UNSPECIFIED., .F., .F.,
 ( 4, 1, 1, 1, 2, 2, 1, 1, 1, 1, 2, 2, 4 ),
 ( 0.000000000000000000, 0.1249999999999810429, 0.1874999999999726608, 0.2187499999999669154, 0.2343749999999659717, 0.2499999999999650280, 0.3749999999999584777, 0.4374999999999563127, 0.4687499999999562572, 0.4843749999999562572, 0.4921874999999562017, 0.4999999999999562572, 1.000000000000000000 ),
 .UNSPECIFIED. ) ;
#8516 = EDGE_LOOP ( 'NONE', ( #3646, #1475 ) ) ;
#8517 = EDGE_CURVE ( 'NONE', #2494, #1934, #3498, .T. ) ;
#8518 = VECTOR ( 'NONE', #8085, 1000.000000000000114 ) ;
#8519 = CARTESIAN_POINT ( 'NONE',  ( -15.65261761014314779, 30.23534695896283253, 53.96687795351272854 ) ) ;
#8520 = ORIENTED_EDGE ( 'NONE', *, *, #8061, .T. ) ;
#8521 = VERTEX_POINT ( 'NONE', #13718 ) ;
#8522 = ORIENTED_EDGE ( 'NONE', *, *, #5865, .T. ) ;
#8523 = PRESENTATION_STYLE_ASSIGNMENT (( #12991 ) ) ;
#8524 = CARTESIAN_POINT ( 'NONE',  ( 140.5320825118609207, 90.00905140961751272, 23.00000000000000000 ) ) ;
#8525 = DIRECTION ( 'NONE',  ( 0.000000000000000000, 0.000000000000000000, -1.000000000000000000 ) ) ;
#8526 = ORIENTED_EDGE ( 'NONE', *, *, #6916, .F. ) ;
#8527 = LINE ( 'NONE', #8661, #6207 ) ;
#8528 = DIRECTION ( 'NONE',  ( 1.000000000000000000, 0.000000000000000000, 0.000000000000000000 ) ) ;
#8529 = EDGE_CURVE ( 'NONE', #10620, #4458, #9972, .T. ) ;
#8530 = DIRECTION ( 'NONE',  ( 0.2148617826751194892, 0.000000000000000000, -0.9766444667050899753 ) ) ;
#8531 = DIRECTION ( 'NONE',  ( 1.000000000000000000, 0.000000000000000000, 0.000000000000000000 ) ) ;
#8532 = MECHANICAL_DESIGN_GEOMETRIC_PRESENTATION_REPRESENTATION (  '', ( #11889 ), #2539 ) ;
#8533 = ORIENTED_EDGE ( 'NONE', *, *, #9228, .T. ) ;
#8534 = CARTESIAN_POINT ( 'NONE',  ( -18.05918829504999934, 10.97290950744599947, 60.60999999999999943 ) ) ;
#8535 = ORIENTED_EDGE ( 'NONE', *, *, #5041, .F. ) ;
#8536 = ORIENTED_EDGE ( 'NONE', *, *, #13214, .T. ) ;
#8537 = VERTEX_POINT ( 'NONE', #8692 ) ;
#8538 = CIRCLE ( 'NONE', #1635, 4.749999999999997335 ) ;
#8539 = LINE ( 'NONE', #8677, #9777 ) ;
#8540 = CARTESIAN_POINT ( 'NONE',  ( -12.26420230435512160, 9.417873376788568507, 64.85000000000000853 ) ) ;
#8541 = ORIENTED_EDGE ( 'NONE', *, *, #11900, .F. ) ;
#8542 = ADVANCED_FACE ( 'NONE', ( #6254 ), #10524, .F. ) ;
#8543 = LINE ( 'NONE', #12744, #916 ) ;
#8544 = CARTESIAN_POINT ( 'NONE',  ( 0.000000000000000000, 0.000000000000000000, 0.000000000000000000 ) ) ;
#8545 = EDGE_CURVE ( 'NONE', #5561, #3266, #5264, .T. ) ;
#8546 = DIRECTION ( 'NONE',  ( 0.000000000000000000, 0.000000000000000000, -1.000000000000000000 ) ) ;
#8547 = CARTESIAN_POINT ( 'NONE',  ( 134.6356359024541973, 94.90549801902425031, 22.75000000000000000 ) ) ;
#8548 = CARTESIAN_POINT ( 'NONE',  ( -18.05918829504999934, 10.97290950744599947, 60.40999999999999659 ) ) ;
#8549 = CONTEXT_DEPENDENT_SHAPE_REPRESENTATION ( #5898, #11060 ) ;
#8550 = CIRCLE ( 'NONE', #531, 34.69999999999999574 ) ;
#8551 = ORIENTED_EDGE ( 'NONE', *, *, #10486, .F. ) ;
#8552 = DIRECTION ( 'NONE',  ( -0.000000000000000000, -0.000000000000000000, 1.000000000000000000 ) ) ;
#8553 = CARTESIAN_POINT ( 'NONE',  ( -36.21615338608749823, 23.36596564213564875, 64.85000000000000853 ) ) ;
#8554 = CYLINDRICAL_SURFACE ( 'NONE', #5363, 0.7500000000000000000 ) ;
#8555 = CARTESIAN_POINT ( 'NONE',  ( 109.0903281124166710, 100.8715034839261762, 10.00000000000000000 ) ) ;
#8556 = CARTESIAN_POINT ( 'NONE',  ( 44.63563590245421153, 85.03908161011132449, 0.3106601717798216367 ) ) ;
#8557 = ORIENTED_EDGE ( 'NONE', *, *, #4412, .T. ) ;
#8558 = LINE ( 'NONE', #2092, #6211 ) ;
#8559 = CARTESIAN_POINT ( 'NONE',  ( -18.88016301897669891, 16.91647750172969822, 68.84999999999999432 ) ) ;
#8560 = DIRECTION ( 'NONE',  ( 1.000000000000000000, 0.000000000000000000, 0.000000000000000000 ) ) ;
#8561 = LINE ( 'NONE', #3276, #3350 ) ;
#8562 = EDGE_CURVE ( 'NONE', #8521, #9884, #8484, .T. ) ;
#8563 = ADVANCED_FACE ( 'NONE', ( #7847 ), #12122, .F. ) ;
#8564 = EDGE_CURVE ( 'NONE', #6589, #8284, #2434, .T. ) ;
#8565 = ORIENTED_EDGE ( 'NONE', *, *, #8478, .F. ) ;
#8566 = ORIENTED_EDGE ( 'NONE', *, *, #5149, .F. ) ;
#8567 = CARTESIAN_POINT ( 'NONE',  ( 44.88563590245420443, 0.000000000000000000, 23.00000000000000000 ) ) ;
#8568 = ORIENTED_EDGE ( 'NONE', *, *, #3059, .T. ) ;
#8569 = EDGE_LOOP ( 'NONE', ( #12137, #2418 ) ) ;
#8570 = CARTESIAN_POINT ( 'NONE',  ( -12.78387628440563084, 8.959369023293000112, 68.21188696640926707 ) ) ;
#8571 = DIRECTION ( 'NONE',  ( -1.000000000000000000, 0.000000000000000000, 0.000000000000000000 ) ) ;
#8572 = LINE ( 'NONE', #11725, #9867 ) ;
#8573 = CARTESIAN_POINT ( 'NONE',  ( -16.02867477244678796, 6.096508287340727250, 68.56773819352413568 ) ) ;
#8574 = CARTESIAN_POINT ( 'NONE',  ( -6.600216501174549499, -2.179141222803650191, 62.14999999999999858 ) ) ;
#8575 = DIRECTION ( 'NONE',  ( 0.000000000000000000, 0.000000000000000000, -1.000000000000000000 ) ) ;
#8576 = EDGE_CURVE ( 'NONE', #7594, #10203, #3534, .T. ) ;
#8577 = AXIS2_PLACEMENT_3D ( 'NONE', #5863, #9019, #12165 ) ;
#8578 = ADVANCED_FACE ( 'NONE', ( #9953 ), #4723, .T. ) ;
#8579 = PRODUCT_DEFINITION_SHAPE ( 'NONE', 'NONE',  #13815 ) ;
#8580 = ORIENTED_EDGE ( 'NONE', *, *, #718, .F. ) ;
#8581 = CARTESIAN_POINT ( 'NONE',  ( -15.53825790700473064, 30.22311051619552558, 54.07754255955762801 ) ) ;
#8582 = ORIENTED_EDGE ( 'NONE', *, *, #66, .F. ) ;
#8583 = ORIENTED_EDGE ( 'NONE', *, *, #9742, .F. ) ;
#8584 = DIRECTION ( 'NONE',  ( 0.000000000000000000, 0.000000000000000000, 1.000000000000000000 ) ) ;
#8585 = AXIS2_PLACEMENT_3D ( 'NONE', #9222, #3977, #7298 ) ;
#8586 = CARTESIAN_POINT ( 'NONE',  ( -12.00918829504999863, 10.97290950744599947, 0.000000000000000000 ) ) ;
#8587 = LINE ( 'NONE', #7666, #2743 ) ;
#8588 = ORIENTED_EDGE ( 'NONE', *, *, #10711, .T. ) ;
#8589 = DIRECTION ( 'NONE',  ( -1.000000000000000000, 5.059610138265691632E-16, 0.000000000000000000 ) ) ;
#8590 = CARTESIAN_POINT ( 'NONE',  ( -18.05918829504999934, 10.97290950744599947, 61.85000000000000142 ) ) ;
#8591 = DIRECTION ( 'NONE',  ( -1.000000000000000000, -0.000000000000000000, -0.000000000000000000 ) ) ;
#8592 = EDGE_CURVE ( 'NONE', #3590, #2432, #372, .T. ) ;
#8593 = FACE_OUTER_BOUND ( 'NONE', #11344, .T. ) ;
#8594 = VECTOR ( 'NONE', #4168, 1000.000000000000000 ) ;
#8595 = EDGE_LOOP ( 'NONE', ( #4477, #11957, #5279, #7513 ) ) ;
#8596 = ORIENTED_EDGE ( 'NONE', *, *, #13245, .F. ) ;
#8597 = ORIENTED_EDGE ( 'NONE', *, *, #7858, .T. ) ;
#8598 = EDGE_CURVE ( 'NONE', #5367, #11674, #6866, .T. ) ;
#8599 = ORIENTED_EDGE ( 'NONE', *, *, #8769, .T. ) ;
#8600 = LINE ( 'NONE', #7609, #6361 ) ;
#8601 = EDGE_LOOP ( 'NONE', ( #10034, #2625, #13688, #13655 ) ) ;
#8602 = ORIENTED_EDGE ( 'NONE', *, *, #7839, .T. ) ;
#8603 = ORIENTED_EDGE ( 'NONE', *, *, #5096, .T. ) ;
#8604 = DIRECTION ( 'NONE',  ( -1.000000000000000000, 0.000000000000000000, 0.000000000000000000 ) ) ;
#8605 = CARTESIAN_POINT ( 'NONE',  ( 44.63563590245420443, 108.9054980190242503, 22.75000000000000000 ) ) ;
#8606 = ORIENTED_EDGE ( 'NONE', *, *, #6896, .F. ) ;
#8607 = CIRCLE ( 'NONE', #3712, 17.00000000000000355 ) ;
#8608 = CARTESIAN_POINT ( 'NONE',  ( -19.55918829504999934, 21.47290950744600124, 57.35000000000000142 ) ) ;
#8609 = CARTESIAN_POINT ( 'NONE',  ( -19.15738950687221731, 26.93589173648236823, 56.32689553783452396 ) ) ;
#8610 = LINE ( 'NONE', #4367, #12662 ) ;
#8611 = DIRECTION ( 'NONE',  ( 0.000000000000000000, 0.000000000000000000, -1.000000000000000000 ) ) ;
#8612 = EDGE_CURVE ( 'NONE', #13530, #6986, #10867, .T. ) ;
#8613 = DIRECTION ( 'NONE',  ( 0.000000000000000000, 0.000000000000000000, -1.000000000000000000 ) ) ;
#8614 = ITEM_DEFINED_TRANSFORMATION ( 'NONE', 'NONE', #875,  #6434 ) ;
#8615 = ORIENTED_EDGE ( 'NONE', *, *, #9571, .T. ) ;
#8616 = EDGE_CURVE ( 'NONE', #7294, #8989, #7471, .T. ) ;
#8617 = VERTEX_POINT ( 'NONE', #1428 ) ;
#8618 = FACE_OUTER_BOUND ( 'NONE', #6045, .T. ) ;
#8619 = CARTESIAN_POINT ( 'NONE',  ( -25.64433075620760150, -3.961216307075045240, 60.65000000000000568 ) ) ;
#8620 = DIRECTION ( 'NONE',  ( -0.9496839325805417342, 0.3132098788326399541, 0.000000000000000000 ) ) ;
#8621 = CARTESIAN_POINT ( 'NONE',  ( 50.53208251186094202, 108.8019446284309737, 23.00000000000000000 ) ) ;
#8622 = CARTESIAN_POINT ( 'NONE',  ( -20.78383927082655092, 30.19994085430307251, 54.29647360000282674 ) ) ;
#8623 = CARTESIAN_POINT ( 'NONE',  ( 3.690811704950004657, 27.97290950744599769, 7.250000000000000000 ) ) ;
#8624 = CARTESIAN_POINT ( 'NONE',  ( -3.743645030049981948, 3.815137874445994282, 61.70038048200006386 ) ) ;
#8625 = LINE ( 'NONE', #8700, #7525 ) ;
#8626 = DIRECTION ( 'NONE',  ( -1.000000000000000000, 0.000000000000000000, 0.000000000000000000 ) ) ;
#8627 = AXIS2_PLACEMENT_3D ( 'NONE', #2733, #6889, #4597 ) ;
#8628 = DIRECTION ( 'NONE',  ( 1.000000000000000000, 0.000000000000000000, 0.000000000000000000 ) ) ;
#8629 = SHAPE_REPRESENTATION_RELATIONSHIP ( 'NONE' , 'NONE' ,  #5502, #9430 ) ;
#8630 = TOROIDAL_SURFACE ( 'NONE', #12216, 3.000000000000000888, 2.000000000000000000 ) ;
#8631 = ORIENTED_EDGE ( 'NONE', *, *, #12200, .T. ) ;
#8632 = CARTESIAN_POINT ( 'NONE',  ( -8.964285665223000521, 0.3335619008453594714, 62.14999999999999858 ) ) ;
#8633 = ORIENTED_EDGE ( 'NONE', *, *, #143, .T. ) ;
#8634 = EDGE_CURVE ( 'NONE', #9938, #10214, #8607, .T. ) ;
#8635 = ORIENTED_EDGE ( 'NONE', *, *, #504, .F. ) ;
#8636 = ORIENTED_EDGE ( 'NONE', *, *, #9034, .F. ) ;
#8637 = FACE_OUTER_BOUND ( 'NONE', #10429, .T. ) ;
#8638 = PRODUCT_DEFINITION_SHAPE ( 'NONE', 'NONE',  #566 ) ;
#8639 = DIRECTION ( 'NONE',  ( -0.4528443260392609471, -0.8915896008669278450, 0.000000000000000000 ) ) ;
#8640 = FACE_OUTER_BOUND ( 'NONE', #988, .T. ) ;
#8641 = CARTESIAN_POINT ( 'NONE',  ( -21.16117192841894834, 4.865520741507539881, 63.64999999999999858 ) ) ;
#8642 = DIRECTION ( 'NONE',  ( 0.000000000000000000, 2.732534507816520408E-15, 1.000000000000000000 ) ) ;
#8643 = CARTESIAN_POINT ( 'NONE',  ( -18.05918829504999934, 10.97290950744599947, 64.85000000000000853 ) ) ;
#8644 = DIRECTION ( 'NONE',  ( 0.4528443260392610026, 0.8915896008669278450, 0.000000000000000000 ) ) ;
#8645 = AXIS2_PLACEMENT_3D ( 'NONE', #6948, #5953, #10175 ) ;
#8646 = VECTOR ( 'NONE', #9522, 1000.000000000000000 ) ;
#8647 = AXIS2_PLACEMENT_3D ( 'NONE', #11965, #6789, #4777 ) ;
#8648 = CARTESIAN_POINT ( 'NONE',  ( -16.24661482249155497, 30.28946906235349346, 53.51494056959690937 ) ) ;
#8649 = ORIENTED_EDGE ( 'NONE', *, *, #1847, .F. ) ;
#8650 = AXIS2_PLACEMENT_3D ( 'NONE', #12432, #11595, #13613 ) ;
#8651 = EDGE_LOOP ( 'NONE', ( #9167, #6739 ) ) ;
#8652 = VECTOR ( 'NONE', #12590, 1000.000000000000000 ) ;
#8653 = CIRCLE ( 'NONE', #5091, 16.72262947720610171 ) ;
#8654 = ADVANCED_FACE ( 'NONE', ( #1283 ), #8827, .T. ) ;
#8655 = ORIENTED_EDGE ( 'NONE', *, *, #10756, .F. ) ;
#8656 = PLANE ( 'NONE',  #4621 ) ;
#8657 = AXIS2_PLACEMENT_3D ( 'NONE', #11548, #11753, #9595 ) ;
#8658 = LINE ( 'NONE', #2405, #7566 ) ;
#8659 = DIRECTION ( 'NONE',  ( 0.6615960714621574867, -0.7498604124941119498, 0.000000000000000000 ) ) ;
#8660 = VERTEX_POINT ( 'NONE', #13163 ) ;
#8661 = CARTESIAN_POINT ( 'NONE',  ( -25.33503448090910126, 29.19143287883919768, 7.250000000000000000 ) ) ;
#8662 = CARTESIAN_POINT ( 'NONE',  ( -14.42040990200814043, 6.848677238728379635, 30.59999999999999787 ) ) ;
#8663 = CARTESIAN_POINT ( 'NONE',  ( 50.63563590245420443, 94.90549801902425031, 23.00000000000000000 ) ) ;
#8664 = CYLINDRICAL_SURFACE ( 'NONE', #1117, 2.000000000000001776 ) ;
#8665 = AXIS2_PLACEMENT_3D ( 'NONE', #6828, #548, #4807 ) ;
#8666 = AXIS2_PLACEMENT_3D ( 'NONE', #8952, #3651, #12162 ) ;
#8667 = AXIS2_PLACEMENT_3D ( 'NONE', #3839, #12484, #2944 ) ;
#8668 = AXIS2_PLACEMENT_3D ( 'NONE', #4141, #8392, #5906 ) ;
#8669 = VERTEX_POINT ( 'NONE', #11076 ) ;
#8670 = ORIENTED_EDGE ( 'NONE', *, *, #10218, .F. ) ;
#8671 = FACE_OUTER_BOUND ( 'NONE', #11189, .T. ) ;
#8672 = ORIENTED_EDGE ( 'NONE', *, *, #7603, .T. ) ;
#8673 = EDGE_CURVE ( 'NONE', #11152, #6401, #378, .T. ) ;
#8674 = VERTEX_POINT ( 'NONE', #9825 ) ;
#8675 = VERTEX_POINT ( 'NONE', #5616 ) ;
#8676 = PRODUCT_DEFINITION_FORMATION_WITH_SPECIFIED_SOURCE ( 'ANY', '', #5400, .NOT_KNOWN. ) ;
#8677 = CARTESIAN_POINT ( 'NONE',  ( -24.03999999999999915, 0.000000000000000000, 7.000000000000000000 ) ) ;
#8678 = FACE_OUTER_BOUND ( 'NONE', #4547, .T. ) ;
#8679 = EDGE_LOOP ( 'NONE', ( #3511, #12610 ) ) ;
#8680 = EDGE_CURVE ( 'NONE', #2763, #11490, #9733, .T. ) ;
#8681 = CARTESIAN_POINT ( 'NONE',  ( -7.499999999999996447, -0.5000000000000019984, -65.00000000000000000 ) ) ;
#8682 = AXIS2_PLACEMENT_3D ( 'NONE', #4286, #138, #10628 ) ;
#8683 = CARTESIAN_POINT ( 'NONE',  ( -16.08092853089235774, 4.500000000000000000, 11.23781208254507469 ) ) ;
#8684 = CARTESIAN_POINT ( 'NONE',  ( -34.65718996104999405, 2.673908674445990119, 63.13003331700004850 ) ) ;
#8685 = AXIS2_PLACEMENT_3D ( 'NONE', #5543, #7476, #1285 ) ;
#8686 = FACE_OUTER_BOUND ( 'NONE', #3810, .T. ) ;
#8687 = EDGE_CURVE ( 'NONE', #4490, #9992, #13637, .T. ) ;
#8688 = DIRECTION ( 'NONE',  ( 0.000000000000000000, 0.000000000000000000, 1.000000000000000000 ) ) ;
#8689 = AXIS2_PLACEMENT_3D ( 'NONE', #12057, #8988, #6878 ) ;
#8690 = ORIENTED_EDGE ( 'NONE', *, *, #816, .T. ) ;
#8691 = EDGE_CURVE ( 'NONE', #8302, #8943, #524, .T. ) ;
#8692 = CARTESIAN_POINT ( 'NONE',  ( -5.309188295050000228, -6.027090492554000534, 64.35000000000000853 ) ) ;
#8693 = DIRECTION ( 'NONE',  ( 1.000000000000000000, 0.000000000000000000, 0.000000000000000000 ) ) ;
#8694 = DIRECTION ( 'NONE',  ( 0.000000000000000000, 0.000000000000000000, 1.000000000000000000 ) ) ;
#8695 = DIRECTION ( 'NONE',  ( 1.000000000000000000, 0.000000000000000000, 0.000000000000000000 ) ) ;
#8696 = CARTESIAN_POINT ( 'NONE',  ( 92.63563590245421153, 99.03908161011133870, -30.00000000000001776 ) ) ;
#8697 = ORIENTED_EDGE ( 'NONE', *, *, #10576, .T. ) ;
#8698 = CARTESIAN_POINT ( 'NONE',  ( -1.059188295049996231, 27.97290950744599769, 68.85549045786049760 ) ) ;
#8699 = DIRECTION ( 'NONE',  ( 0.000000000000000000, 0.000000000000000000, 1.000000000000000000 ) ) ;
#8700 = CARTESIAN_POINT ( 'NONE',  ( 44.63563590245421864, 85.03908161011133870, 19.25000000000000000 ) ) ;
#8701 = CARTESIAN_POINT ( 'NONE',  ( -18.05918829504999934, 10.97290950744599947, 68.84999999999999432 ) ) ;
#8702 = ADVANCED_FACE ( 'NONE', ( #9894 ), #319, .T. ) ;
#8703 = ORIENTED_EDGE ( 'NONE', *, *, #6604, .F. ) ;
#8704 = DIRECTION ( 'NONE',  ( -0.000000000000000000, -0.000000000000000000, -1.000000000000000000 ) ) ;
#8705 = AXIS2_PLACEMENT_3D ( 'NONE', #11228, #6816, #11996 ) ;
#8706 = CONICAL_SURFACE ( 'NONE', #9162, 5.000000000000000888, 0.7853981633974497223 ) ;
#8707 = VECTOR ( 'NONE', #9738, 1000.000000000000000 ) ;
#8708 = VERTEX_POINT ( 'NONE', #12952 ) ;
#8709 = ORIENTED_EDGE ( 'NONE', *, *, #2366, .F. ) ;
#8710 = EDGE_LOOP ( 'NONE', ( #1369, #4107 ) ) ;
#8711 = AXIS2_PLACEMENT_3D ( 'NONE', #10155, #8694, #1214 ) ;
#8712 = DIRECTION ( 'NONE',  ( -0.000000000000000000, -0.000000000000000000, -1.000000000000000000 ) ) ;
#8713 = AXIS2_PLACEMENT_3D ( 'NONE', #5903, #8854, #8084 ) ;
#8714 = CIRCLE ( 'NONE', #1579, 23.22993838181874793 ) ;
#8715 = CIRCLE ( 'NONE', #6701, 10.00000000000000178 ) ;
#8716 = EDGE_LOOP ( 'NONE', ( #3558, #1889 ) ) ;
#8717 = ORIENTED_EDGE ( 'NONE', *, *, #5418, .T. ) ;
#8718 = DIRECTION ( 'NONE',  ( 1.000000000000000000, 1.577021341797097560E-16, -0.000000000000000000 ) ) ;
#8719 = CARTESIAN_POINT ( 'NONE',  ( 81.82136590429890077, 114.1051029460540605, 10.00000000000000000 ) ) ;
#8720 = CARTESIAN_POINT ( 'NONE',  ( 50.63563590245420443, 108.9054980190242503, 20.00000000000000000 ) ) ;
#8721 = DIRECTION ( 'NONE',  ( 0.000000000000000000, 0.000000000000000000, 1.000000000000000000 ) ) ;
#8722 = CARTESIAN_POINT ( 'NONE',  ( -18.05918829504999934, 10.00028003023991907, 63.45000000000000284 ) ) ;
#8723 = DIRECTION ( 'NONE',  ( 0.000000000000000000, 0.000000000000000000, 1.000000000000000000 ) ) ;
#8724 = ADVANCED_FACE ( 'NONE', ( #8906 ), #11139, .F. ) ;
#8725 = LINE ( 'NONE', #11794, #7642 ) ;
#8726 = CYLINDRICAL_SURFACE ( 'NONE', #8430, 2.700000000000001066 ) ;
#8727 = AXIS2_PLACEMENT_3D ( 'NONE', #8238, #11518, #9291 ) ;
#8728 = VECTOR ( 'NONE', #12868, 1000.000000000000000 ) ;
#8729 = AXIS2_PLACEMENT_3D ( 'NONE', #1089, #7640, #8560 ) ;
#8730 = VERTEX_POINT ( 'NONE', #9506 ) ;
#8731 = CARTESIAN_POINT ( 'NONE',  ( -15.29419851136037067, 30.19514031481103089, 54.34376022666191375 ) ) ;
#8732 = VERTEX_POINT ( 'NONE', #12261 ) ;
#8733 = CYLINDRICAL_SURFACE ( 'NONE', #7059, 6.000000000000000888 ) ;
#8734 = MECHANICAL_DESIGN_GEOMETRIC_PRESENTATION_REPRESENTATION (  '', ( #9412 ), #255 ) ;
#8735 = CARTESIAN_POINT ( 'NONE',  ( -30.32854245105399826, 27.54455229823479812, 64.85000000000000853 ) ) ;
#8736 = CIRCLE ( 'NONE', #10525, 6.345833333000001630 ) ;
#8737 = CYLINDRICAL_SURFACE ( 'NONE', #10290, 0.2500000000000002220 ) ;
#8738 = ORIENTED_EDGE ( 'NONE', *, *, #7825, .F. ) ;
#8739 = AXIS2_PLACEMENT_3D ( 'NONE', #7341, #11631, #12401 ) ;
#8740 = FACE_OUTER_BOUND ( 'NONE', #10807, .T. ) ;
#8741 = CARTESIAN_POINT ( 'NONE',  ( -18.05918829504999223, 19.18892026044601096, 63.36264408500002787 ) ) ;
#8742 = CARTESIAN_POINT ( 'NONE',  ( -39.30918829504999934, 27.97290950744599769, 64.35000000000000853 ) ) ;
#8743 = ADVANCED_FACE ( 'NONE', ( #9374 ), #11602, .T. ) ;
#8744 = EDGE_CURVE ( 'NONE', #2573, #8804, #4164, .T. ) ;
#8745 = ORIENTED_EDGE ( 'NONE', *, *, #1465, .F. ) ;
#8746 = DIRECTION ( 'NONE',  ( 0.000000000000000000, 0.000000000000000000, -1.000000000000000000 ) ) ;
#8747 = VERTEX_POINT ( 'NONE', #12514 ) ;
#8748 = ORIENTED_EDGE ( 'NONE', *, *, #11776, .T. ) ;
#8749 = ORIENTED_EDGE ( 'NONE', *, *, #4794, .F. ) ;
#8750 = ADVANCED_BREP_SHAPE_REPRESENTATION ( '', ( #4352, #9410, #4601, #5147, #5212, #229, #13799, #6434 ), #5097 ) ;
#8751 = ORIENTED_EDGE ( 'NONE', *, *, #1487, .T. ) ;
#8752 = EDGE_LOOP ( 'NONE', ( #12589, #11249, #6169, #2604 ) ) ;
#8753 = CARTESIAN_POINT ( 'NONE',  ( -4.059188295049996675, 27.97290950744599769, 0.000000000000000000 ) ) ;
#8754 = DIRECTION ( 'NONE',  ( 0.000000000000000000, 0.000000000000000000, 1.000000000000000000 ) ) ;
#8755 = ORIENTED_EDGE ( 'NONE', *, *, #11243, .F. ) ;
#8756 = CARTESIAN_POINT ( 'NONE',  ( 20.45469220996244175, 1.832421873814834123, -3.000000000000000000 ) ) ;
#8757 = DIRECTION ( 'NONE',  ( -1.000000000000000000, 0.000000000000000000, 0.000000000000000000 ) ) ;
#8758 = CARTESIAN_POINT ( 'NONE',  ( -18.05918829504999934, 10.97290950744599947, 14.00000000000000000 ) ) ;
#8759 = CARTESIAN_POINT ( 'NONE',  ( 116.7775623211734342, 123.0390816101113245, 0.7500000000000006661 ) ) ;
#8760 = DIRECTION ( 'NONE',  ( -1.000000000000000000, 0.000000000000000000, 0.000000000000000000 ) ) ;
#8761 = EDGE_CURVE ( 'NONE', #4325, #6311, #2973, .T. ) ;
#8762 = ORIENTED_EDGE ( 'NONE', *, *, #5832, .F. ) ;
#8763 = ADVANCED_FACE ( 'NONE', ( #8388 ), #13750, .T. ) ;
#8764 = CIRCLE ( 'NONE', #2320, 23.49999999999999645 ) ;
#8765 = ORIENTED_EDGE ( 'NONE', *, *, #9182, .T. ) ;
#8766 = ORIENTED_EDGE ( 'NONE', *, *, #4918, .F. ) ;
#8767 = EDGE_CURVE ( 'NONE', #2349, #4357, #5888, .T. ) ;
#8768 = DIRECTION ( 'NONE',  ( 0.000000000000000000, 0.000000000000000000, -1.000000000000000000 ) ) ;
#8769 = EDGE_CURVE ( 'NONE', #11310, #2183, #7388, .T. ) ;
#8770 = DIRECTION ( 'NONE',  ( 0.000000000000000000, 0.000000000000000000, 1.000000000000000000 ) ) ;
#8771 = CARTESIAN_POINT ( 'NONE',  ( -18.05918829504999934, 10.97290950744599947, 27.09999999999999787 ) ) ;
#8772 = CARTESIAN_POINT ( 'NONE',  ( -19.71007448221605074, 30.30175501178326414, 53.41939229818840573 ) ) ;
#8773 = B_SPLINE_CURVE_WITH_KNOTS ( 'NONE', 3,
 ( #9525, #10717, #90, #7339, #2009, #8609, #4366, #5196, #6380, #12604, #7409, #3056, #11552, #6241, #13710, #4157, #8405, #12673, #3125, #11629, #1005, #4427, #4502, #5667, #10018, #6523, #373, #10788, #1203, #7684, #8820, #10931, #7764, #8894, #1484, #10858, #7618, #11969, #6733 ),
 .UNSPECIFIED., .F., .F.,
 ( 4, 2, 2, 2, 2, 1, 1, 2, 2, 2, 2, 2, 2, 2, 1, 1, 1, 2, 2, 2, 2, 4 ),
 ( 0.000000000000000000, 0.1250000000000901501, 0.1875000000001344480, 0.2187500000001581513, 0.2343750000001693645, 0.2421875000001743050, 0.2460937500001758038, 0.2480468750001765255, 0.2500000000001772471, 0.3750000000001733058, 0.5000000000001693090, 0.6250000000001654232, 0.6875000000001656453, 0.7187500000001668665, 0.7343750000001686429, 0.7421875000001706413, 0.7460937500001703082, 0.7480468750001699751, 0.7500000000001697531, 0.8125000000001261213, 0.8750000000000824896, 1.000000000000000000 ),
 .UNSPECIFIED. ) ;
#8774 = DIRECTION ( 'NONE',  ( 0.000000000000000000, 0.000000000000000000, -1.000000000000000000 ) ) ;
#8775 = ORIENTED_EDGE ( 'NONE', *, *, #6086, .F. ) ;
#8776 = CARTESIAN_POINT ( 'NONE',  ( -3.531395436049983960, 18.23680593644601089, 62.03182374100001084 ) ) ;
#8777 = FACE_BOUND ( 'NONE', #6246, .T. ) ;
#8778 = LINE ( 'NONE', #262, #8056 ) ;
#8779 = VECTOR ( 'NONE', #2982, 1000.000000000000000 ) ;
#8780 = DIRECTION ( 'NONE',  ( -0.000000000000000000, -0.000000000000000000, -1.000000000000000000 ) ) ;
#8781 = ADVANCED_FACE ( 'NONE', ( #4206 ), #8452, .T. ) ;
#8782 = EDGE_LOOP ( 'NONE', ( #7882, #8844, #8566, #4798, #3115, #12855, #12255, #11801 ) ) ;
#8783 = EDGE_CURVE ( 'NONE', #665, #4627, #10169, .T. ) ;
#8784 = CYLINDRICAL_SURFACE ( 'NONE', #10618, 6.000000000000000888 ) ;
#8785 = ORIENTED_EDGE ( 'NONE', *, *, #8093, .F. ) ;
#8786 = DIRECTION ( 'NONE',  ( 0.08563346120589268584, 0.000000000000000000, -0.9963267086261908823 ) ) ;
#8787 = CARTESIAN_POINT ( 'NONE',  ( -7.499999999999996447, -0.5000000000000017764, -65.00000000000000000 ) ) ;
#8788 = DIRECTION ( 'NONE',  ( 1.000000000000000000, 0.000000000000000000, 0.000000000000000000 ) ) ;
#8789 = DIRECTION ( 'NONE',  ( 0.000000000000000000, 0.000000000000000000, 1.000000000000000000 ) ) ;
#8790 = CARTESIAN_POINT ( 'NONE',  ( 0.000000000000000000, 8.500000000000000000, -13.50000000000000000 ) ) ;
#8791 = DIRECTION ( 'NONE',  ( 0.000000000000000000, 1.000000000000000000, -0.000000000000000000 ) ) ;
#8792 = DIRECTION ( 'NONE',  ( -0.000000000000000000, -0.000000000000000000, -1.000000000000000000 ) ) ;
#8793 = FACE_OUTER_BOUND ( 'NONE', #7649, .T. ) ;
#8794 = CARTESIAN_POINT ( 'NONE',  ( -30.80918829504999934, -6.027090492554000534, 64.85000000000000853 ) ) ;
#8795 = ADVANCED_FACE ( 'NONE', ( #9106 ), #12651, .T. ) ;
#8796 = EDGE_CURVE ( 'NONE', #13262, #11891, #4611, .T. ) ;
#8797 = ORIENTED_EDGE ( 'NONE', *, *, #13338, .T. ) ;
#8798 = EDGE_CURVE ( 'NONE', #13076, #13640, #840, .T. ) ;
#8799 = ORIENTED_EDGE ( 'NONE', *, *, #7012, .T. ) ;
#8800 = CARTESIAN_POINT ( 'NONE',  ( -15.41280400920135030, 7.973467857469549891, 30.59999999999999787 ) ) ;
#8801 = CARTESIAN_POINT ( 'NONE',  ( 0.000000000000000000, 0.000000000000000000, -23.49999999999999645 ) ) ;
#8802 = CARTESIAN_POINT ( 'NONE',  ( 109.1537879975201406, 115.4601262030644762, 0.7500000000000006661 ) ) ;
#8803 = DIRECTION ( 'NONE',  ( 0.6615960714621574867, -0.7498604124941119498, 0.000000000000000000 ) ) ;
#8804 = VERTEX_POINT ( 'NONE', #5105 ) ;
#8805 = CYLINDRICAL_SURFACE ( 'NONE', #13138, 0.7500000000000072164 ) ;
#8806 = DIRECTION ( 'NONE',  ( 0.000000000000000000, 0.000000000000000000, -1.000000000000000000 ) ) ;
#8807 = DIRECTION ( 'NONE',  ( -8.673617379884027583E-16, -1.000000000000000000, 0.000000000000000000 ) ) ;
#8808 = CLOSED_SHELL ( 'NONE', ( #10669, #801, #10399, #13700, #6562, #3581 ) ) ;
#8809 = VERTEX_POINT ( 'NONE', #11529 ) ;
#8810 = VECTOR ( 'NONE', #5592, 1000.000000000000000 ) ;
#8811 = ORIENTED_EDGE ( 'NONE', *, *, #986, .F. ) ;
#8812 = FACE_OUTER_BOUND ( 'NONE', #11044, .T. ) ;
#8813 = ORIENTED_EDGE ( 'NONE', *, *, #5160, .T. ) ;
#8814 = ORIENTED_EDGE ( 'NONE', *, *, #5261, .F. ) ;
#8815 = ORIENTED_EDGE ( 'NONE', *, *, #6135, .F. ) ;
#8816 = DIRECTION ( 'NONE',  ( 0.000000000000000000, 0.000000000000000000, -1.000000000000000000 ) ) ;
#8817 = ADVANCED_FACE ( 'NONE', ( #1978 ), #5175, .T. ) ;
#8818 = CARTESIAN_POINT ( 'NONE',  ( -12.04995946920099925, -4.929579886311989512, 62.14999999999999858 ) ) ;
#8819 = FACE_OUTER_BOUND ( 'NONE', #12135, .T. ) ;
#8820 = CARTESIAN_POINT ( 'NONE',  ( -17.19771031368804515, 26.94970066966654798, 56.12204914942099521 ) ) ;
#8821 = FACE_OUTER_BOUND ( 'NONE', #9068, .T. ) ;
#8822 = AXIS2_PLACEMENT_3D ( 'NONE', #8632, #4385, #1163 ) ;
#8823 = DIRECTION ( 'NONE',  ( -0.000000000000000000, -0.000000000000000000, 1.000000000000000000 ) ) ;
#8824 = ORIENTED_EDGE ( 'NONE', *, *, #4989, .F. ) ;
#8825 = VERTEX_POINT ( 'NONE', #4135 ) ;
#8826 = AXIS2_PLACEMENT_3D ( 'NONE', #13450, #10255, #1931 ) ;
#8827 = CYLINDRICAL_SURFACE ( 'NONE', #1482, 16.95000000000000284 ) ;
#8828 = ORIENTED_EDGE ( 'NONE', *, *, #8942, .T. ) ;
#8829 = LINE ( 'NONE', #6007, #4828 ) ;
#8830 = ORIENTED_EDGE ( 'NONE', *, *, #4185, .T. ) ;
#8831 = EDGE_CURVE ( 'NONE', #5137, #13422, #13297, .T. ) ;
#8832 = CARTESIAN_POINT ( 'NONE',  ( -30.30918829504999934, -6.027090492554000534, 68.85549045786049760 ) ) ;
#8833 = CARTESIAN_POINT ( 'NONE',  ( -20.92870944094807584, 30.18239061225282427, 60.22698406536613192 ) ) ;
#8834 = FACE_OUTER_BOUND ( 'NONE', #10969, .T. ) ;
#8835 = VERTEX_POINT ( 'NONE', #989 ) ;
#8836 = LINE ( 'NONE', #6672, #13800 ) ;
#8837 = CARTESIAN_POINT ( 'NONE',  ( 5.640422211807141650, 16.89844320975774750, 0.000000000000000000 ) ) ;
#8838 = DIRECTION ( 'NONE',  ( -0.7091883091770476710, -0.7050191076322684935, 0.000000000000000000 ) ) ;
#8839 = CARTESIAN_POINT ( 'NONE',  ( -14.95720466168106100, 17.08029827338444662, 64.54999999999999716 ) ) ;
#8840 = AXIS2_PLACEMENT_3D ( 'NONE', #6216, #9446, #13690 ) ;
#8841 = ORIENTED_EDGE ( 'NONE', *, *, #10756, .T. ) ;
#8842 = EDGE_LOOP ( 'NONE', ( #8869, #932, #5285, #12784 ) ) ;
#8843 = DIRECTION ( 'NONE',  ( 0.000000000000000000, 0.000000000000000000, -1.000000000000000000 ) ) ;
#8844 = ORIENTED_EDGE ( 'NONE', *, *, #4399, .F. ) ;
#8845 = APPLICATION_CONTEXT ( 'automotive_design' ) ;
#8846 = DIRECTION ( 'NONE',  ( -1.000000000000000000, 0.000000000000000000, -0.000000000000000000 ) ) ;
#8847 = ORIENTED_EDGE ( 'NONE', *, *, #1648, .T. ) ;
#8848 = ORIENTED_EDGE ( 'NONE', *, *, #8102, .F. ) ;
#8849 = DIRECTION ( 'NONE',  ( -1.000000000000000000, 0.000000000000000000, 0.000000000000000000 ) ) ;
#8850 = EDGE_CURVE ( 'NONE', #12622, #5356, #6298, .T. ) ;
#8851 = CARTESIAN_POINT ( 'NONE',  ( -5.789834139046019956, -5.598733283342819611, 68.85549045786049760 ) ) ;
#8852 = CIRCLE ( 'NONE', #6830, 6.449999999999997513 ) ;
#8853 = CARTESIAN_POINT ( 'NONE',  ( 16.08092853089229024, 4.500000000000000000, -9.237812082545193704 ) ) ;
#8854 = DIRECTION ( 'NONE',  ( 0.000000000000000000, 0.000000000000000000, 1.000000000000000000 ) ) ;
#8855 = ORIENTED_EDGE ( 'NONE', *, *, #4968, .T. ) ;
#8856 = FACE_BOUND ( 'NONE', #7261, .T. ) ;
#8857 = FACE_OUTER_BOUND ( 'NONE', #8448, .T. ) ;
#8858 = DIRECTION ( 'NONE',  ( 1.000000000000000000, 0.000000000000000000, 0.000000000000000000 ) ) ;
#8859 = EDGE_CURVE ( 'NONE', #13545, #10605, #5236, .T. ) ;
#8860 = DIRECTION ( 'NONE',  ( 0.000000000000000000, 0.000000000000000000, -1.000000000000000000 ) ) ;
#8861 = CARTESIAN_POINT ( 'NONE',  ( 2.262399129208275017, -0.4981161769137599782, 17.25000000000000000 ) ) ;
#8862 = ADVANCED_FACE ( 'NONE', ( #1110 ), #13060, .T. ) ;
#8863 = ORIENTED_EDGE ( 'NONE', *, *, #8316, .T. ) ;
#8864 = ORIENTED_EDGE ( 'NONE', *, *, #8796, .F. ) ;
#8865 = CARTESIAN_POINT ( 'NONE',  ( 42.63563590245419732, 111.0390816101113103, 0.3106601717798218587 ) ) ;
#8866 = VERTEX_POINT ( 'NONE', #5370 ) ;
#8867 = ORIENTED_EDGE ( 'NONE', *, *, #13528, .F. ) ;
#8869 = ORIENTED_EDGE ( 'NONE', *, *, #4879, .T. ) ;
#8868 = EDGE_CURVE ( 'NONE', #6506, #13804, #2336, .T. ) ;
#8870 = CYLINDRICAL_SURFACE ( 'NONE', #2412, 4.749999999999997335 ) ;
#8871 = CARTESIAN_POINT ( 'NONE',  ( 100.2760581142613603, 115.9375248198690826, 10.00000000000000000 ) ) ;
#8872 = VECTOR ( 'NONE', #2356, 1000.000000000000000 ) ;
#8873 = CARTESIAN_POINT ( 'NONE',  ( 92.63563590245421153, 112.2890816101113387, 19.25000000000000000 ) ) ;
#8874 = AXIS2_PLACEMENT_3D ( 'NONE', #2577, #12129, #5752 ) ;
#8875 = DIRECTION ( 'NONE',  ( 1.000000000000000000, 0.000000000000000000, 0.000000000000000000 ) ) ;
#8876 = CIRCLE ( 'NONE', #10427, 4.250000000000000000 ) ;
#8877 = CARTESIAN_POINT ( 'NONE',  ( 42.63563590245419732, 111.0390816101113387, 19.25000000000000000 ) ) ;
#8878 = EDGE_CURVE ( 'NONE', #6060, #1530, #4824, .T. ) ;
#8879 = PLANE ( 'NONE',  #8042 ) ;
#8880 = AXIS2_PLACEMENT_3D ( 'NONE', #5861, #6068, #8444 ) ;
#8881 = AXIS2_PLACEMENT_3D ( 'NONE', #8853, #3563, #8927 ) ;
#8882 = AXIS2_PLACEMENT_3D ( 'NONE', #12288, #1452, #1387 ) ;
#8883 = EDGE_LOOP ( 'NONE', ( #2184, #11692, #6576, #6195 ) ) ;
#8884 = AXIS2_PLACEMENT_3D ( 'NONE', #11481, #10305, #4990 ) ;
#8885 = EDGE_LOOP ( 'NONE', ( #3034, #10105, #7547, #11212 ) ) ;
#8886 = CARTESIAN_POINT ( 'NONE',  ( -17.01567291573902807, 30.33713881007578195, 61.54486793806091782 ) ) ;
#8887 = EDGE_LOOP ( 'NONE', ( #6498, #7239 ) ) ;
#8888 = VERTEX_POINT ( 'NONE', #5302 ) ;
#8889 = ORIENTED_EDGE ( 'NONE', *, *, #9178, .F. ) ;
#8890 = DIRECTION ( 'NONE',  ( -0.000000000000000000, 1.000000000000000000, -0.000000000000000000 ) ) ;
#8891 = CARTESIAN_POINT ( 'NONE',  ( 105.4499059006094654, 83.97306027416853169, 10.00000000000000000 ) ) ;
#8892 = ORIENTED_EDGE ( 'NONE', *, *, #2614, .T. ) ;
#8893 = CARTESIAN_POINT ( 'NONE',  ( 0.4408117049500004381, 10.97290950744600124, 12.50000000000000000 ) ) ;
#8894 = CARTESIAN_POINT ( 'NONE',  ( -16.99569662973183171, 26.93820700769395771, 56.28689761106198119 ) ) ;
#8895 = AXIS2_PLACEMENT_3D ( 'NONE', #12174, #2626, #1555 ) ;
#8896 = CIRCLE ( 'NONE', #11790, 3.450000000000001510 ) ;
#8897 = CYLINDRICAL_SURFACE ( 'NONE', #8917, 3.000000000000001332 ) ;
#8898 = CIRCLE ( 'NONE', #6203, 17.00000000000000355 ) ;
#8899 = EDGE_CURVE ( 'NONE', #1219, #318, #10629, .T. ) ;
#8900 = DIRECTION ( 'NONE',  ( 1.000000000000000000, 0.000000000000000000, 0.000000000000000000 ) ) ;
#8901 = ORIENTED_EDGE ( 'NONE', *, *, #4393, .T. ) ;
#8902 = CARTESIAN_POINT ( 'NONE',  ( -16.41522250449391152, 5.755460197997838812, 68.40012421657081632 ) ) ;
#8903 = EDGE_LOOP ( 'NONE', ( #858, #1337, #13689, #3513 ) ) ;
#8904 = ORIENTED_EDGE ( 'NONE', *, *, #12720, .F. ) ;
#8905 = CIRCLE ( 'NONE', #3123, 17.00000000000000355 ) ;
#8906 = FACE_OUTER_BOUND ( 'NONE', #12106, .T. ) ;
#8907 = CARTESIAN_POINT ( 'NONE',  ( 16.08092853089229024, 4.500000000000000000, -7.237812082545199921 ) ) ;
#8908 = CARTESIAN_POINT ( 'NONE',  ( -21.29754790531509201, 30.13344396834369832, 55.03342513115495649 ) ) ;
#8909 =( BOUNDED_CURVE ( )  B_SPLINE_CURVE ( 3, ( #4888, #1736, #13533, #7233 ),
 .UNSPECIFIED., .F., .F. ) 
 B_SPLINE_CURVE_WITH_KNOTS ( ( 4, 4 ),
 ( 1.570796326794896558, 3.141592653589793116 ),
 .UNSPECIFIED. ) 
 CURVE ( )  GEOMETRIC_REPRESENTATION_ITEM ( )  RATIONAL_B_SPLINE_CURVE ( ( 1.000000000000000000, 0.8047378541243649375, 0.8047378541243649375, 1.000000000000000000 ) ) 
 REPRESENTATION_ITEM ( '' )  );
#8910 = DIRECTION ( 'NONE',  ( -0.000000000000000000, -0.000000000000000000, -1.000000000000000000 ) ) ;
#8911 = ORIENTED_EDGE ( 'NONE', *, *, #5230, .F. ) ;
#8912 = DIRECTION ( 'NONE',  ( 0.7071067811865500152, 0.000000000000000000, 0.7071067811865450192 ) ) ;
#8913 = CARTESIAN_POINT ( 'NONE',  ( -18.05918829504999934, 10.97290950744599947, 60.04999999999999716 ) ) ;
#8914 = CARTESIAN_POINT ( 'NONE',  ( 86.63563590245421153, 99.03908161011133870, -30.00000000000001776 ) ) ;
#8915 = CARTESIAN_POINT ( 'NONE',  ( -18.05918829504999934, 10.97290950744599947, 57.35000000000000142 ) ) ;
#8916 = ORIENTED_EDGE ( 'NONE', *, *, #3026, .T. ) ;
#8917 = AXIS2_PLACEMENT_3D ( 'NONE', #12179, #11135, #313 ) ;
#8918 = CIRCLE ( 'NONE', #4466, 2.000000000000001776 ) ;
#8919 = EDGE_CURVE ( 'NONE', #5925, #68, #2399, .T. ) ;
#8920 = EDGE_CURVE ( 'NONE', #13687, #2345, #12417, .T. ) ;
#8921 = ORIENTED_EDGE ( 'NONE', *, *, #4456, .T. ) ;
#8922 = LINE ( 'NONE', #4532, #10842 ) ;
#8923 = FACE_OUTER_BOUND ( 'NONE', #12931, .T. ) ;
#8924 = EDGE_LOOP ( 'NONE', ( #8911, #9821, #11246, #10465 ) ) ;
#8925 = CARTESIAN_POINT ( 'NONE',  ( -16.45469220996245596, -1.832421873814834123, -3.000000000000000000 ) ) ;
#8926 = PLANE ( 'NONE',  #1953 ) ;
#8927 = DIRECTION ( 'NONE',  ( 0.000000000000000000, 0.000000000000000000, 1.000000000000000000 ) ) ;
#8928 = FACE_OUTER_BOUND ( 'NONE', #9100, .T. ) ;
#8929 = AXIS2_PLACEMENT_3D ( 'NONE', #8170, #9075, #12374 ) ;
#8930 = AXIS2_PLACEMENT_3D ( 'NONE', #11357, #13579, #5894 ) ;
#8931 = CARTESIAN_POINT ( 'NONE',  ( -3.999999999999997335, 2.000000000000000000, -65.00000000000000000 ) ) ;
#8932 = DIRECTION ( 'NONE',  ( 0.000000000000000000, 0.000000000000000000, 1.000000000000000000 ) ) ;
#8933 = DIRECTION ( 'NONE',  ( 0.000000000000000000, 0.000000000000000000, 1.000000000000000000 ) ) ;
#8934 = CARTESIAN_POINT ( 'NONE',  ( 134.8856359024541973, 0.000000000000000000, 22.75000000000000000 ) ) ;
#8935 = CARTESIAN_POINT ( 'NONE',  ( -3.125062480528954634, 3.387767046288379991, 58.54999999999999716 ) ) ;
#8936 = B_SPLINE_CURVE_WITH_KNOTS ( 'NONE', 3,
 ( #9455, #11409, #9312, #13561, #8186, #12595, #8394, #3043, #1695, #12660, #11539, #10230, #6999, #10497, #647, #12451, #5185, #13697 ),
 .UNSPECIFIED., .F., .F.,
 ( 4, 2, 2, 2, 2, 2, 2, 2, 4 ),
 ( 0.000000000000000000, 0.1250000000000000000, 0.2500000000000000000, 0.3750000000000000000, 0.5000000000000000000, 0.6250000000000000000, 0.7500000000000000000, 0.8750000000000000000, 1.000000000000000000 ),
 .UNSPECIFIED. ) ;
#8937 = CARTESIAN_POINT ( 'NONE',  ( -18.05918829430470041, 19.27290950744890097, 63.15000000009349179 ) ) ;
#8938 = EDGE_CURVE ( 'NONE', #8958, #3979, #6563, .T. ) ;
#8939 = AXIS2_PLACEMENT_3D ( 'NONE', #8871, #208, #7738 ) ;
#8940 = AXIS2_PLACEMENT_3D ( 'NONE', #10630, #10567, #995 ) ;
#8941 = EDGE_LOOP ( 'NONE', ( #8116, #13487 ) ) ;
#8942 = EDGE_CURVE ( 'NONE', #3923, #8965, #1248, .T. ) ;
#8943 = VERTEX_POINT ( 'NONE', #9786 ) ;
#8944 = VERTEX_POINT ( 'NONE', #9652 ) ;
#8945 = LINE ( 'NONE', #9925, #355 ) ;
#8946 = MANIFOLD_SOLID_BREP ( 'Boss-Extrude1', #8808 ) ;
#8947 = VERTEX_POINT ( 'NONE', #8801 ) ;
#8948 = EDGE_LOOP ( 'NONE', ( #2332, #9379, #10925, #6683 ) ) ;
#8949 = ADVANCED_FACE ( 'NONE', ( #6707 ), #8733, .T. ) ;
#8950 = CARTESIAN_POINT ( 'NONE',  ( 140.5069562460138286, 85.34974178189114014, 2.445552345904828725E-16 ) ) ;
#8951 = DIRECTION ( 'NONE',  ( 1.000000000000000000, 0.000000000000000000, 0.000000000000000000 ) ) ;
#8952 = CARTESIAN_POINT ( 'NONE',  ( 0.000000000000000000, 0.000000000000000000, 17.25000000000000000 ) ) ;
#8953 = CIRCLE ( 'NONE', #2949, 18.00000000000000000 ) ;
#8954 = AXIS2_PLACEMENT_3D ( 'NONE', #7009, #7995, #4658 ) ;
#8955 = FACE_OUTER_BOUND ( 'NONE', #9671, .T. ) ;
#8956 = CARTESIAN_POINT ( 'NONE',  ( 50.63563590245420443, 103.9054980190242361, 23.00000000000000000 ) ) ;
#8957 = EDGE_CURVE ( 'NONE', #2414, #8660, #598, .T. ) ;
#8958 = VERTEX_POINT ( 'NONE', #10694 ) ;
#8959 = CYLINDRICAL_SURFACE ( 'NONE', #1216, 1.500000000000001332 ) ;
#8960 = AXIS2_PLACEMENT_3D ( 'NONE', #6050, #1801, #8357 ) ;
#8961 = VECTOR ( 'NONE', #3199, 1000.000000000000000 ) ;
#8962 = ORIENTED_EDGE ( 'NONE', *, *, #10641, .T. ) ;
#8963 = ORIENTED_EDGE ( 'NONE', *, *, #2330, .T. ) ;
#8964 = ADVANCED_FACE ( 'NONE', ( #69 ), #8656, .T. ) ;
#8965 = VERTEX_POINT ( 'NONE', #6500 ) ;
#8966 = DIRECTION ( 'NONE',  ( -0.000000000000000000, -0.000000000000000000, -1.000000000000000000 ) ) ;
#8967 = EDGE_LOOP ( 'NONE', ( #335, #11328, #1971, #953, #3400, #4420, #2518, #9585, #3245, #1231, #10845, #12718, #6801 ) ) ;
#8968 = DIRECTION ( 'NONE',  ( 0.000000000000000000, 0.000000000000000000, 1.000000000000000000 ) ) ;
#8969 = ORIENTED_EDGE ( 'NONE', *, *, #9657, .F. ) ;
#8970 = CARTESIAN_POINT ( 'NONE',  ( -18.05918829504999934, 10.97290950744599947, 64.85000000000000853 ) ) ;
#8971 = CARTESIAN_POINT ( 'NONE',  ( -16.04064420431702942, 4.500000000000000000, -11.30758658292224439 ) ) ;
#8972 = DIRECTION ( 'NONE',  ( 0.000000000000000000, 0.000000000000000000, -1.000000000000000000 ) ) ;
#8973 = FACE_OUTER_BOUND ( 'NONE', #495, .T. ) ;
#8974 = EDGE_LOOP ( 'NONE', ( #2977, #3113, #1506, #7962 ) ) ;
#8975 = EDGE_CURVE ( 'NONE', #12380, #13076, #3580, .T. ) ;
#8976 = VERTEX_POINT ( 'NONE', #1535 ) ;
#8977 = ORIENTED_EDGE ( 'NONE', *, *, #4254, .F. ) ;
#8978 = EDGE_CURVE ( 'NONE', #5838, #6577, #3357, .T. ) ;
#8979 = CIRCLE ( 'NONE', #11428, 3.800000000000002487 ) ;
#8980 = CARTESIAN_POINT ( 'NONE',  ( 44.63563590245419732, 108.9054980190242503, 22.89644660940672694 ) ) ;
#8981 = ORIENTED_EDGE ( 'NONE', *, *, #4118, .F. ) ;
#8982 = DIRECTION ( 'NONE',  ( 1.000000000000000000, 0.000000000000000000, 0.000000000000000000 ) ) ;
#8983 = CARTESIAN_POINT ( 'NONE',  ( -21.03590444521807967, 30.16892808484258737, 54.61432211296680350 ) ) ;
#8984 =( LENGTH_UNIT ( ) NAMED_UNIT ( * ) SI_UNIT ( .MILLI., .METRE. ) );
#8985 = DIRECTION ( 'NONE',  ( 0.6615960714621574867, -0.7498604124941119498, 0.000000000000000000 ) ) ;
#8986 = LINE ( 'NONE', #3475, #2894 ) ;
#8987 = DIRECTION ( 'NONE',  ( 0.000000000000000000, 0.000000000000000000, -1.000000000000000000 ) ) ;
#8988 = DIRECTION ( 'NONE',  ( 0.000000000000000000, 0.000000000000000000, -1.000000000000000000 ) ) ;
#8989 = VERTEX_POINT ( 'NONE', #11109 ) ;
#8990 = AXIS2_PLACEMENT_3D ( 'NONE', #5393, #12869, #2141 ) ;
#8991 =( BOUNDED_CURVE ( )  B_SPLINE_CURVE ( 3, ( #7041, #10550, #12643, #4128 ),
 .UNSPECIFIED., .F., .F. ) 
 B_SPLINE_CURVE_WITH_KNOTS ( ( 4, 4 ),
 ( 0.000000000000000000, 1.570796326794896558 ),
 .UNSPECIFIED. ) 
 CURVE ( )  GEOMETRIC_REPRESENTATION_ITEM ( )  RATIONAL_B_SPLINE_CURVE ( ( 1.000000000000000000, 0.8047378541243649375, 0.8047378541243649375, 1.000000000000000000 ) ) 
 REPRESENTATION_ITEM ( '' )  );
#8992 = LINE ( 'NONE', #6815, #9280 ) ;
#8993 = DIRECTION ( 'NONE',  ( 0.000000000000000000, 0.000000000000000000, 1.000000000000000000 ) ) ;
#8994 = ORIENTED_EDGE ( 'NONE', *, *, #4768, .F. ) ;
#8995 = CARTESIAN_POINT ( 'NONE',  ( 50.63563590245420443, 108.9054980190242503, 22.75000000000000000 ) ) ;
#8996 = DIRECTION ( 'NONE',  ( 0.000000000000000000, 0.000000000000000000, -1.000000000000000000 ) ) ;
#8997 = CARTESIAN_POINT ( 'NONE',  ( -7.241070169793059286, 29.81324547859994922, 17.25000000000000000 ) ) ;
#8998 = CONICAL_SURFACE ( 'NONE', #2552, 4.250000000000000000, 0.7853981633974524978 ) ;
#8999 = CARTESIAN_POINT ( 'NONE',  ( -25.64433075620760150, -3.961216307075045240, 58.54999999999999716 ) ) ;
#9000 = CYLINDRICAL_SURFACE ( 'NONE', #7379, 1.999999999999995781 ) ;
#9001 = LINE ( 'NONE', #4677, #1080 ) ;
#9002 = CYLINDRICAL_SURFACE ( 'NONE', #10006, 16.95000000000000284 ) ;
#9003 = ADVANCED_FACE ( 'NONE', ( #2753 ), #8870, .T. ) ;
#9004 = FACE_OUTER_BOUND ( 'NONE', #10674, .T. ) ;
#9005 = CARTESIAN_POINT ( 'NONE',  ( 4.000000000000001776, -4.336808689942017736E-16, -65.00000000000000000 ) ) ;
#9006 = CARTESIAN_POINT ( 'NONE',  ( -1.396365658198039927, 10.97290950744599947, 17.25000000000000000 ) ) ;
#9007 = AXIS2_PLACEMENT_3D ( 'NONE', #11165, #547, #1390 ) ;
#9008 = VERTEX_POINT ( 'NONE', #2545 ) ;
#9009 = EDGE_LOOP ( 'NONE', ( #10137, #9589, #3591, #7845 ) ) ;
#9010 = EDGE_LOOP ( 'NONE', ( #12477, #5082, #3518, #8451 ) ) ;
#9011 = FACE_OUTER_BOUND ( 'NONE', #10472, .T. ) ;
#9012 = CARTESIAN_POINT ( 'NONE',  ( -35.05918829505000645, -6.027090492554000534, 5.250000000000000000 ) ) ;
#9013 = CARTESIAN_POINT ( 'NONE',  ( -1.059188295049996231, 27.97290950744599769, 0.000000000000000000 ) ) ;
#9014 = DIRECTION ( 'NONE',  ( 0.000000000000000000, 0.000000000000000000, -1.000000000000000000 ) ) ;
#9015 = EDGE_CURVE ( 'NONE', #13437, #5856, #11974, .T. ) ;
#9016 = DIRECTION ( 'NONE',  ( 1.000000000000000000, 0.000000000000000000, 0.000000000000000000 ) ) ;
#9017 = DIRECTION ( 'NONE',  ( 0.000000000000000000, 0.000000000000000000, -1.000000000000000000 ) ) ;
#9018 = ADVANCED_FACE ( 'NONE', ( #1607 ), #5715, .F. ) ;
#9019 = DIRECTION ( 'NONE',  ( 0.000000000000000000, 0.000000000000000000, -1.000000000000000000 ) ) ;
#9020 = ORIENTED_EDGE ( 'NONE', *, *, #8139, .F. ) ;
#9021 = ORIENTED_EDGE ( 'NONE', *, *, #9638, .F. ) ;
#9022 = ORIENTED_EDGE ( 'NONE', *, *, #4814, .T. ) ;
#9023 = CARTESIAN_POINT ( 'NONE',  ( -16.56453087281537861, 30.31214524168932201, 61.35958320581661951 ) ) ;
#9024 = EDGE_LOOP ( 'NONE', ( #11617, #8179, #6003, #11542 ) ) ;
#9025 = ORIENTED_EDGE ( 'NONE', *, *, #6115, .F. ) ;
#9026 = FACE_BOUND ( 'NONE', #12336, .T. ) ;
#9027 = DIRECTION ( 'NONE',  ( 0.000000000000000000, 0.000000000000000000, 1.000000000000000000 ) ) ;
#9028 = CARTESIAN_POINT ( 'NONE',  ( 44.94629607423406270, 112.2890816101113387, 0.000000000000000000 ) ) ;
#9029 = EDGE_CURVE ( 'NONE', #12630, #10544, #1039, .T. ) ;
#9030 = ORIENTED_EDGE ( 'NONE', *, *, #5908, .F. ) ;
#9031 = DIRECTION ( 'NONE',  ( 1.000000000000000000, 0.000000000000000000, 0.000000000000000000 ) ) ;
#9032 = DIRECTION ( 'NONE',  ( 0.000000000000000000, 0.000000000000000000, -1.000000000000000000 ) ) ;
#9033 = DIRECTION ( 'NONE',  ( 0.000000000000000000, 0.000000000000000000, 1.000000000000000000 ) ) ;
#9034 = EDGE_CURVE ( 'NONE', #12138, #3128, #6774, .T. ) ;
#9035 = DIRECTION ( 'NONE',  ( -1.000000000000000000, 0.000000000000000000, 0.000000000000000000 ) ) ;
#9036 = ADVANCED_FACE ( 'NONE', ( #13407 ), #9977, .T. ) ;
#9037 = CIRCLE ( 'NONE', #7674, 13.50000000000000000 ) ;
#9038 = VERTEX_POINT ( 'NONE', #1672 ) ;
#9039 = CARTESIAN_POINT ( 'NONE',  ( -11.74835982676941981, -4.028726038184999858, 62.14999999999999858 ) ) ;
#9040 = PLANE ( 'NONE',  #2647 ) ;
#9041 = ADVANCED_FACE ( 'NONE', ( #12367 ), #7949, .F. ) ;
#9042 = VECTOR ( 'NONE', #9355, 1000.000000000000114 ) ;
#9043 = CARTESIAN_POINT ( 'NONE',  ( -21.62809706959791356, 30.08448262671908324, 58.92298932101692088 ) ) ;
#9044 = PLANE ( 'NONE',  #4092 ) ;
#9045 = DIRECTION ( 'NONE',  ( 0.000000000000000000, 0.000000000000000000, -1.000000000000000000 ) ) ;
#9046 = DIRECTION ( 'NONE',  ( 0.000000000000000000, 0.000000000000000000, -1.000000000000000000 ) ) ;
#9047 = CARTESIAN_POINT ( 'NONE',  ( -24.06841712089904917, -4.929579886311989512, 62.14999999999999858 ) ) ;
#9048 = DIRECTION ( 'NONE',  ( 1.000000000000000000, 0.000000000000000000, 0.000000000000000000 ) ) ;
#9049 = ADVANCED_FACE ( 'NONE', ( #554 ), #8401, .T. ) ;
#9050 = VECTOR ( 'NONE', #8142, 1000.000000000000000 ) ;
#9051 = DIRECTION ( 'NONE',  ( 0.000000000000000000, 0.000000000000000000, -1.000000000000000000 ) ) ;
#9052 = DIRECTION ( 'NONE',  ( 0.000000000000000000, 0.000000000000000000, 1.000000000000000000 ) ) ;
#9053 = FACE_OUTER_BOUND ( 'NONE', #7255, .T. ) ;
#9054 = CARTESIAN_POINT ( 'NONE',  ( 92.63563590245421153, 99.03908161011133870, 0.7500000000000006661 ) ) ;
#9055 = DIRECTION ( 'NONE',  ( 0.000000000000000000, 0.000000000000000000, -1.000000000000000000 ) ) ;
#9056 = CARTESIAN_POINT ( 'NONE',  ( -22.99102692894637556, 13.28949390873614078, 68.40321543070255927 ) ) ;
#9057 = CARTESIAN_POINT ( 'NONE',  ( -18.05918829504999934, 10.97290950744599947, 64.85000000000000853 ) ) ;
#9058 = CARTESIAN_POINT ( 'NONE',  ( -7.241070169793070832, 29.81324547859995278, 83.57661607529820458 ) ) ;
#9059 = CARTESIAN_POINT ( 'NONE',  ( 8.500000000000003553, 2.499999999999999556, -65.00000000000000000 ) ) ;
#9060 = VECTOR ( 'NONE', #3736, 1000.000000000000000 ) ;
#9061 = CARTESIAN_POINT ( 'NONE',  ( 10.81426999815522549, -15.06602133594279991, 0.000000000000000000 ) ) ;
#9062 = DIRECTION ( 'NONE',  ( 1.000000000000000000, 0.000000000000000000, 0.000000000000000000 ) ) ;
#9063 = ORIENTED_EDGE ( 'NONE', *, *, #12666, .F. ) ;
#9064 = EDGE_CURVE ( 'NONE', #6077, #12460, #6945, .T. ) ;
#9065 = CIRCLE ( 'NONE', #3283, 16.95000000000000284 ) ;
#9066 = ORIENTED_EDGE ( 'NONE', *, *, #5510, .T. ) ;
#9067 = DIRECTION ( 'NONE',  ( 0.000000000000000000, 0.000000000000000000, 1.000000000000000000 ) ) ;
#9068 = EDGE_LOOP ( 'NONE', ( #550, #8814, #12538, #5119 ) ) ;
#9069 = VERTEX_POINT ( 'NONE', #4893 ) ;
#9070 = DIRECTION ( 'NONE',  ( 0.000000000000000000, 0.000000000000000000, -1.000000000000000000 ) ) ;
#9071 = DIRECTION ( 'NONE',  ( 0.000000000000000000, 0.000000000000000000, -1.000000000000000000 ) ) ;
#9072 = LINE ( 'NONE', #357, #2962 ) ;
#9073 = CARTESIAN_POINT ( 'NONE',  ( -4.599650328638321461, 8.500000000000001776, -9.878124499050784380 ) ) ;
#9074 = CARTESIAN_POINT ( 'NONE',  ( 86.63563590245421153, 99.03908161011133870, 20.00000000000000000 ) ) ;
#9075 = DIRECTION ( 'NONE',  ( -1.000000000000000000, 0.000000000000000000, 0.000000000000000000 ) ) ;
#9076 = VECTOR ( 'NONE', #6048, 1000.000000000000000 ) ;
#9077 = CARTESIAN_POINT ( 'NONE',  ( -18.05918829504999934, 28.64232754551664684, 58.85000000000000142 ) ) ;
#9078 = EDGE_CURVE ( 'NONE', #6986, #3428, #3077, .T. ) ;
#9079 = ORIENTED_EDGE ( 'NONE', *, *, #7390, .T. ) ;
#9080 = EDGE_CURVE ( 'NONE', #13429, #12769, #8852, .T. ) ;
#9081 = ORIENTED_EDGE ( 'NONE', *, *, #2892, .F. ) ;
#9082 = ORIENTED_EDGE ( 'NONE', *, *, #3935, .F. ) ;
#9083 = CARTESIAN_POINT ( 'NONE',  ( -8.930582367738718830, 12.35910059330153921, 64.85000000000000853 ) ) ;
#9084 = ADVANCED_FACE ( 'NONE', ( #8103 ), #354, .F. ) ;
#9085 = ORIENTED_EDGE ( 'NONE', *, *, #10564, .F. ) ;
#9086 = VECTOR ( 'NONE', #10730, 1000.000000000000000 ) ;
#9087 = FACE_BOUND ( 'NONE', #4441, .T. ) ;
#9088 = VERTEX_POINT ( 'NONE', #4756 ) ;
#9089 = DIRECTION ( 'NONE',  ( -1.000000000000000000, 0.000000000000000000, 0.000000000000000000 ) ) ;
#9090 = CARTESIAN_POINT ( 'NONE',  ( -18.05918829504999934, 10.97290950744599947, 5.250000000000000000 ) ) ;
#9091 = CARTESIAN_POINT ( 'NONE',  ( -23.24102627739274851, -6.265087914666300328, 62.14999999999999858 ) ) ;
#9092 = DIRECTION ( 'NONE',  ( 0.000000000000000000, 0.000000000000000000, -1.000000000000000000 ) ) ;
#9093 = CARTESIAN_POINT ( 'NONE',  ( 2.262399129208274129, 22.44393519180576746, 5.250000000000000000 ) ) ;
#9094 = EDGE_CURVE ( 'NONE', #12141, #10905, #6398, .T. ) ;
#9095 = DIRECTION ( 'NONE',  ( 0.000000000000000000, 0.000000000000000000, -1.000000000000000000 ) ) ;
#9096 = DIRECTION ( 'NONE',  ( 0.000000000000000000, -1.000000000000000000, 0.000000000000000000 ) ) ;
#9097 = AXIS2_PLACEMENT_3D ( 'NONE', #1037, #5432, #8644 ) ;
#9098 = CIRCLE ( 'NONE', #13119, 2.999999999999999112 ) ;
#9099 = CIRCLE ( 'NONE', #4653, 1.999999999999991340 ) ;
#9100 = EDGE_LOOP ( 'NONE', ( #7079, #4810, #5222, #1228 ) ) ;
#9101 = EDGE_CURVE ( 'NONE', #12100, #11802, #9065, .T. ) ;
#9102 = EDGE_CURVE ( 'NONE', #956, #4939, #6159, .T. ) ;
#9103 = ORIENTED_EDGE ( 'NONE', *, *, #6239, .T. ) ;
#9104 = ORIENTED_EDGE ( 'NONE', *, *, #2700, .F. ) ;
#9105 = ADVANCED_FACE ( 'NONE', ( #5019 ), #6062, .F. ) ;
#9106 = FACE_OUTER_BOUND ( 'NONE', #12533, .T. ) ;
#9107 = ORIENTED_EDGE ( 'NONE', *, *, #7725, .F. ) ;
#9108 = CIRCLE ( 'NONE', #3773, 4.250000000000000000 ) ;
#9109 = AXIS2_PLACEMENT_3D ( 'NONE', #11062, #1478, #5728 ) ;
#9110 = CIRCLE ( 'NONE', #12681, 4.750000000000000888 ) ;
#9111 = CARTESIAN_POINT ( 'NONE',  ( -0.04028432657539327000, 4.500000000000000000, 20.54539866546728888 ) ) ;
#9112 = AXIS2_PLACEMENT_3D ( 'NONE', #5306, #12591, #3182 ) ;
#9113 = EDGE_CURVE ( 'NONE', #755, #8462, #11522, .T. ) ;
#9114 = CARTESIAN_POINT ( 'NONE',  ( -21.28806243134481591, 30.13477816395881703, 55.01643572729695109 ) ) ;
#9115 = EDGE_CURVE ( 'NONE', #10360, #8485, #2177, .T. ) ;
#9116 = DIRECTION ( 'NONE',  ( 1.000000000000000000, 0.000000000000000000, 0.000000000000000000 ) ) ;
#9117 = FACE_OUTER_BOUND ( 'NONE', #5800, .T. ) ;
#9118 = DIRECTION ( 'NONE',  ( -0.000000000000000000, -0.000000000000000000, 1.000000000000000000 ) ) ;
#9119 = DIRECTION ( 'NONE',  ( -1.000000000000000000, 0.000000000000000000, 0.000000000000000000 ) ) ;
#9120 = PRODUCT_CONTEXT ( 'NONE', #9304, 'mechanical' ) ;
#9121 = PRODUCT_DEFINITION_FORMATION_WITH_SPECIFIED_SOURCE ( 'ANY', '', #10774, .NOT_KNOWN. ) ;
#9122 = VECTOR ( 'NONE', #5860, 1000.000000000000000 ) ;
#9123 = CIRCLE ( 'NONE', #1533, 6.000000000000005329 ) ;
#9124 = EDGE_CURVE ( 'NONE', #721, #5520, #12705, .T. ) ;
#9125 = CIRCLE ( 'NONE', #7741, 34.70000000000000284 ) ;
#9126 = EDGE_CURVE ( 'NONE', #9069, #6829, #10864, .T. ) ;
#9127 = CARTESIAN_POINT ( 'NONE',  ( -14.32322260522609980, 18.32852371459815188, 63.64999999999999858 ) ) ;
#9128 = CARTESIAN_POINT ( 'NONE',  ( 81.82136590429890077, 114.1051029460540605, 20.00000000000000000 ) ) ;
#9129 = ORIENTED_EDGE ( 'NONE', *, *, #5812, .F. ) ;
#9130 = FACE_OUTER_BOUND ( 'NONE', #13144, .T. ) ;
#9131 = DIRECTION ( 'NONE',  ( 0.000000000000000000, 0.000000000000000000, 1.000000000000000000 ) ) ;
#9132 = ADVANCED_FACE ( 'NONE', ( #11451 ), #10545, .F. ) ;
#9133 = FACE_OUTER_BOUND ( 'NONE', #10256, .T. ) ;
#9134 = FACE_OUTER_BOUND ( 'NONE', #787, .T. ) ;
#9135 = CARTESIAN_POINT ( 'NONE',  ( -35.05918829505000645, 10.97290950744599947, 64.35000000000000853 ) ) ;
#9136 = CARTESIAN_POINT ( 'NONE',  ( 72.18094369249178044, 97.20665973629650125, 20.00000000000000000 ) ) ;
#9137 = FACE_OUTER_BOUND ( 'NONE', #2798, .T. ) ;
#9138 = DIRECTION ( 'NONE',  ( 0.000000000000000000, 0.000000000000000000, 1.000000000000000000 ) ) ;
#9139 = DIRECTION ( 'NONE',  ( 0.000000000000000000, 1.000000000000000000, 0.000000000000000000 ) ) ;
#9140 = CIRCLE ( 'NONE', #2246, 0.9499999999999995115 ) ;
#9141 = DIRECTION ( 'NONE',  ( 0.000000000000000000, 1.000000000000000000, 0.000000000000000000 ) ) ;
#9142 = ORIENTED_EDGE ( 'NONE', *, *, #5478, .F. ) ;
#9143 = ORIENTED_EDGE ( 'NONE', *, *, #8783, .F. ) ;
#9144 = VERTEX_POINT ( 'NONE', #13536 ) ;
#9145 = AXIS2_PLACEMENT_3D ( 'NONE', #1829, #13542, #12433 ) ;
#9146 = ORIENTED_EDGE ( 'NONE', *, *, #345, .T. ) ;
#9147 = DIRECTION ( 'NONE',  ( 0.4528443260392610026, 0.8915896008669278450, 0.000000000000000000 ) ) ;
#9148 = ORIENTED_EDGE ( 'NONE', *, *, #234, .T. ) ;
#9149 = AXIS2_PLACEMENT_3D ( 'NONE', #8548, #2081, #10647 ) ;
#9150 = VERTEX_POINT ( 'NONE', #3981 ) ;
#9151 = ORIENTED_EDGE ( 'NONE', *, *, #4536, .T. ) ;
#9152 = CARTESIAN_POINT ( 'NONE',  ( 103.4499059006094512, 83.97306027416853169, 20.00000000000000000 ) ) ;
#9153 = EDGE_CURVE ( 'NONE', #6090, #12804, #4390, .T. ) ;
#9154 = CARTESIAN_POINT ( 'NONE',  ( 103.4499059006094512, 83.97306027416853169, 10.00000000000000000 ) ) ;
#9155 = DIRECTION ( 'NONE',  ( 0.000000000000000000, 1.000000000000000000, -0.000000000000000000 ) ) ;
#9156 = LINE ( 'NONE', #9999, #13797 ) ;
#9157 = CARTESIAN_POINT ( 'NONE',  ( -18.05918829504999223, 2.756898754446003963, 63.36264408500002787 ) ) ;
#9158 = FACE_OUTER_BOUND ( 'NONE', #1617, .T. ) ;
#9159 = DIRECTION ( 'NONE',  ( 1.000000000000000000, 0.000000000000000000, 0.000000000000000000 ) ) ;
#9160 = AXIS2_PLACEMENT_3D ( 'NONE', #399, #336, #4671 ) ;
#9161 =( BOUNDED_CURVE ( )  B_SPLINE_CURVE ( 3, ( #2975, #843, #7123, #7189 ),
 .UNSPECIFIED., .F., .F. ) 
 B_SPLINE_CURVE_WITH_KNOTS ( ( 4, 4 ),
 ( 0.06314145700000579897, 0.9368585430000010428 ),
 .UNSPECIFIED. ) 
 CURVE ( )  GEOMETRIC_REPRESENTATION_ITEM ( )  RATIONAL_B_SPLINE_CURVE ( ( 0.9565783021659900465, 0.7697947703959749921, 0.7697947703959759913, 0.9565783021659940433 ) ) 
 REPRESENTATION_ITEM ( '' )  );
#9162 = AXIS2_PLACEMENT_3D ( 'NONE', #2546, #6775, #4064 ) ;
#9163 = CIRCLE ( 'NONE', #13175, 6.449999999999997513 ) ;
#9164 = ORIENTED_EDGE ( 'NONE', *, *, #7879, .T. ) ;
#9165 = DIRECTION ( 'NONE',  ( -1.000000000000000000, -0.000000000000000000, -0.000000000000000000 ) ) ;
#9166 = ORIENTED_EDGE ( 'NONE', *, *, #9571, .F. ) ;
#9167 = ORIENTED_EDGE ( 'NONE', *, *, #9218, .F. ) ;
#9168 = FACE_OUTER_BOUND ( 'NONE', #12118, .T. ) ;
#9169 = CIRCLE ( 'NONE', #2950, 0.9499999999999995115 ) ;
#9170 = PLANE ( 'NONE',  #905 ) ;
#9171 = ORIENTED_EDGE ( 'NONE', *, *, #8375, .T. ) ;
#9172 = AXIS2_PLACEMENT_3D ( 'NONE', #4805, #5845, #8427 ) ;
#9173 = EDGE_LOOP ( 'NONE', ( #13601, #9476, #11245, #6144 ) ) ;
#9174 = CARTESIAN_POINT ( 'NONE',  ( -18.05918829505001355, 3.709013078446008027, 62.03182374100007479 ) ) ;
#9175 = CARTESIAN_POINT ( 'NONE',  ( -6.000000000000000888, -12.00000000000000178, 7.000000000000000000 ) ) ;
#9176 = DIRECTION ( 'NONE',  ( 0.000000000000000000, -1.000000000000000000, 0.000000000000000000 ) ) ;
#9177 = CARTESIAN_POINT ( 'NONE',  ( 116.7775623211734342, 75.03908161011133870, 0.7500000000000006661 ) ) ;
#9178 = EDGE_CURVE ( 'NONE', #13218, #1212, #7485, .T. ) ;
#9179 = DIRECTION ( 'NONE',  ( -0.000000000000000000, -0.000000000000000000, 1.000000000000000000 ) ) ;
#9180 = EDGE_CURVE ( 'NONE', #1281, #1970, #8515, .T. ) ;
#9181 = CARTESIAN_POINT ( 'NONE',  ( -35.05918829505000645, 27.97290950744599769, 17.25000000000000000 ) ) ;
#9182 = EDGE_CURVE ( 'NONE', #5000, #13550, #12199, .T. ) ;
#9183 = MECHANICAL_DESIGN_GEOMETRIC_PRESENTATION_REPRESENTATION (  '', ( #7156 ), #486 ) ;
#9184 = AXIS2_PLACEMENT_3D ( 'NONE', #7408, #11755, #11696 ) ;
#9185 = CIRCLE ( 'NONE', #3831, 7.150000000000001243 ) ;
#9186 = ORIENTED_EDGE ( 'NONE', *, *, #507, .T. ) ;
#9187 = ORIENTED_EDGE ( 'NONE', *, *, #11704, .T. ) ;
#9188 = ORIENTED_EDGE ( 'NONE', *, *, #1770, .F. ) ;
#9189 = DIRECTION ( 'NONE',  ( -0.8915896008669277339, 0.4528443260392608916, 0.000000000000000000 ) ) ;
#9190 = CARTESIAN_POINT ( 'NONE',  ( 7.500000000000000000, -0.5000000000000017764, 0.000000000000000000 ) ) ;
#9191 = AXIS2_PLACEMENT_3D ( 'NONE', #120, #10548, #2108 ) ;
#9192 = FACE_BOUND ( 'NONE', #2299, .T. ) ;
#9193 = FACE_OUTER_BOUND ( 'NONE', #1493, .T. ) ;
#9194 = DIRECTION ( 'NONE',  ( 0.000000000000000000, 1.000000000000000000, 0.000000000000000000 ) ) ;
#9195 = EDGE_CURVE ( 'NONE', #8965, #2082, #7265, .T. ) ;
#9196 = CARTESIAN_POINT ( 'NONE',  ( 27.50000000000001066, 0.000000000000000000, -30.00000000000000355 ) ) ;
#9197 = APPLICATION_PROTOCOL_DEFINITION ( 'draft international standard', 'automotive_design', 1998, #4761 ) ;
#9198 = EDGE_CURVE ( 'NONE', #3141, #6919, #12645, .T. ) ;
#9199 = ORIENTED_EDGE ( 'NONE', *, *, #9452, .T. ) ;
#9200 = ADVANCED_FACE ( 'NONE', ( #6552 ), #118, .T. ) ;
#9201 = CIRCLE ( 'NONE', #951, 12.00000000000000355 ) ;
#9202 = LINE ( 'NONE', #1867, #9050 ) ;
#9203 = EDGE_LOOP ( 'NONE', ( #435, #5231, #4449, #11783 ) ) ;
#9204 = ORIENTED_EDGE ( 'NONE', *, *, #12256, .F. ) ;
#9205 = DIRECTION ( 'NONE',  ( 0.000000000000000000, 0.000000000000000000, -1.000000000000000000 ) ) ;
#9206 = CARTESIAN_POINT ( 'NONE',  ( -18.05918829504999934, 10.97290950744599947, 64.35000000000000853 ) ) ;
#9207 = CARTESIAN_POINT ( 'NONE',  ( -10.25088531517540069, -8.860076549334108265, 5.250000000000000000 ) ) ;
#9208 = CARTESIAN_POINT ( 'NONE',  ( -18.05918829504999934, 10.97290950744599947, 64.85000000000000853 ) ) ;
#9209 = CARTESIAN_POINT ( 'NONE',  ( -25.32001676333059947, -4.028726038184999858, 63.45000000000000284 ) ) ;
#9210 = CARTESIAN_POINT ( 'NONE',  ( 44.63563590245419732, 103.9054980190242361, 22.89644660940672694 ) ) ;
#9211 = CARTESIAN_POINT ( 'NONE',  ( -18.05918829504999934, 10.97290950744599947, 58.35000000000000142 ) ) ;
#9212 = STYLED_ITEM ( 'NONE', ( #990 ), #348 ) ;
#9213 = DIRECTION ( 'NONE',  ( 0.000000000000000000, 0.000000000000000000, -1.000000000000000000 ) ) ;
#9214 = EDGE_CURVE ( 'NONE', #11089, #8282, #6402, .T. ) ;
#9215 = AXIS2_PLACEMENT_3D ( 'NONE', #7992, #5891, #10174 ) ;
#9216 = FACE_OUTER_BOUND ( 'NONE', #6941, .T. ) ;
#9217 = PRODUCT_DEFINITION_CONTEXT ( 'detailed design', #4054, 'design' ) ;
#9218 = EDGE_CURVE ( 'NONE', #4939, #956, #13756, .T. ) ;
#9219 = EDGE_LOOP ( 'NONE', ( #2990, #2521, #1882, #7536 ) ) ;
#9220 = AXIS2_PLACEMENT_3D ( 'NONE', #2838, #1694, #8050 ) ;
#9221 = EDGE_LOOP ( 'NONE', ( #1702, #13473, #8690, #1458 ) ) ;
#9222 = CARTESIAN_POINT ( 'NONE',  ( -7.999999999999998224, 2.000000000000000000, -65.00000000000000000 ) ) ;
#9223 = EDGE_LOOP ( 'NONE', ( #12663, #3222, #4384, #11885 ) ) ;
#9224 = DIRECTION ( 'NONE',  ( 1.000000000000000000, 0.000000000000000000, 0.000000000000000000 ) ) ;
#9225 = CYLINDRICAL_SURFACE ( 'NONE', #12728, 4.250000000000000000 ) ;
#9226 = CARTESIAN_POINT ( 'NONE',  ( -18.05918829504999934, 10.97290950744599947, 56.84999999999999432 ) ) ;
#9227 = CARTESIAN_POINT ( 'NONE',  ( -23.49332020752115113, 0.2738342970428629952, 57.35000000000000142 ) ) ;
#9228 = EDGE_CURVE ( 'NONE', #12616, #7297, #1306, .T. ) ;
#9229 = CARTESIAN_POINT ( 'NONE',  ( 6.940811704950001548, 32.97290950744599769, 0.000000000000000000 ) ) ;
#9230 = PLANE ( 'NONE',  #10480 ) ;
#9231 = CARTESIAN_POINT ( 'NONE',  ( -5.631644894983189431, 10.97290950744599947, 7.250000000000000000 ) ) ;
#9232 = CIRCLE ( 'NONE', #744, 17.00000000000000355 ) ;
#9233 = EDGE_CURVE ( 'NONE', #9852, #9150, #8190, .T. ) ;
#9234 = ORIENTED_EDGE ( 'NONE', *, *, #13366, .F. ) ;
#9235 = ORIENTED_EDGE ( 'NONE', *, *, #9892, .F. ) ;
#9236 = CARTESIAN_POINT ( 'NONE',  ( -15.80158631607083564, 30.25033399978765658, 60.86361540000825698 ) ) ;
#9237 = VERTEX_POINT ( 'NONE', #6483 ) ;
#9238 = EDGE_LOOP ( 'NONE', ( #8097, #4339 ) ) ;
#9239 =( LENGTH_UNIT ( ) NAMED_UNIT ( * ) SI_UNIT ( .MILLI., .METRE. ) );
#9240 = CARTESIAN_POINT ( 'NONE',  ( -18.05918829505000289, 3.688421942730967906, 61.99499741764299898 ) ) ;
#9241 = ORIENTED_EDGE ( 'NONE', *, *, #2542, .F. ) ;
#9242 = VERTEX_POINT ( 'NONE', #55 ) ;
#9243 = DIRECTION ( 'NONE',  ( 0.000000000000000000, 0.000000000000000000, -1.000000000000000000 ) ) ;
#9244 = DIRECTION ( 'NONE',  ( 1.000000000000000000, 0.000000000000000000, 0.000000000000000000 ) ) ;
#9245 = EDGE_LOOP ( 'NONE', ( #4277, #3614, #8520, #4061 ) ) ;
#9246 = CARTESIAN_POINT ( 'NONE',  ( -6.600216501174579697, -2.179141222803619993, 63.45000000000000284 ) ) ;
#9247 = LINE ( 'NONE', #3875, #6542 ) ;
#9248 = CARTESIAN_POINT ( 'NONE',  ( -35.05918829505000645, -6.027090492554000534, 64.35000000000000853 ) ) ;
#9249 = CARTESIAN_POINT ( 'NONE',  ( 134.6356359024541973, 108.9054980190242503, 23.00000000000000000 ) ) ;
#9250 = EDGE_CURVE ( 'NONE', #2367, #5154, #10751, .T. ) ;
#9251 = ORIENTED_EDGE ( 'NONE', *, *, #9113, .T. ) ;
#9252 = ORIENTED_EDGE ( 'NONE', *, *, #10202, .F. ) ;
#9253 = EDGE_CURVE ( 'NONE', #13005, #12066, #10419, .T. ) ;
#9254 = ORIENTED_EDGE ( 'NONE', *, *, #2548, .T. ) ;
#9255 = CARTESIAN_POINT ( 'NONE',  ( 3.940811704950009542, -14.02709049255400053, 10.00000000000000000 ) ) ;
#9256 = DIRECTION ( 'NONE',  ( -0.6615960714621568206, 0.7498604124941127269, 0.000000000000000000 ) ) ;
#9257 = DIRECTION ( 'NONE',  ( -0.000000000000000000, 1.000000000000000000, -0.000000000000000000 ) ) ;
#9258 = FACE_OUTER_BOUND ( 'NONE', #9426, .T. ) ;
#9259 = DIRECTION ( 'NONE',  ( 0.000000000000000000, 0.000000000000000000, -1.000000000000000000 ) ) ;
#9260 = AXIS2_PLACEMENT_3D ( 'NONE', #12929, #11893, #3381 ) ;
#9261 = DIRECTION ( 'NONE',  ( 0.000000000000000000, 0.000000000000000000, 1.000000000000000000 ) ) ;
#9262 = APPLICATION_PROTOCOL_DEFINITION ( 'draft international standard', 'automotive_design', 1998, #8845 ) ;
#9263 = ORIENTED_EDGE ( 'NONE', *, *, #8356, .T. ) ;
#9264 = EDGE_CURVE ( 'NONE', #2555, #8732, #12898, .T. ) ;
#9265 = ORIENTED_EDGE ( 'NONE', *, *, #9178, .T. ) ;
#9266 = AXIS2_PLACEMENT_3D ( 'NONE', #4613, #6833, #10984 ) ;
#9267 = DIRECTION ( 'NONE',  ( -0.000000000000000000, -0.000000000000000000, -1.000000000000000000 ) ) ;
#9268 = ORIENTED_EDGE ( 'NONE', *, *, #1917, .T. ) ;
#9269 = ORIENTED_EDGE ( 'NONE', *, *, #1949, .F. ) ;
#9270 = CARTESIAN_POINT ( 'NONE',  ( -28.87730642030695094, -7.867426463707980488, 17.25000000000000000 ) ) ;
#9271 = FACE_OUTER_BOUND ( 'NONE', #13324, .T. ) ;
#9272 = CARTESIAN_POINT ( 'NONE',  ( -7.999999999999998224, 2.000000000000000000, -65.00000000000000000 ) ) ;
#9273 = CARTESIAN_POINT ( 'NONE',  ( -22.82340340075558771, 13.43738685772752994, 68.48657388181956662 ) ) ;
#9274 = CARTESIAN_POINT ( 'NONE',  ( -18.05918829504999934, 19.07290950615085023, 63.35000000000700027 ) ) ;
#9275 = DIRECTION ( 'NONE',  ( 1.000000000000000000, 0.000000000000000000, 0.000000000000000000 ) ) ;
#9276 = DIRECTION ( 'NONE',  ( 0.000000000000000000, 1.000000000000000000, -0.000000000000000000 ) ) ;
#9277 = LINE ( 'NONE', #1946, #7413 ) ;
#9278 = CARTESIAN_POINT ( 'NONE',  ( 6.940811704950009542, -11.02709049255400053, 0.000000000000000000 ) ) ;
#9279 = AXIS2_PLACEMENT_3D ( 'NONE', #8453, #12586, #10623 ) ;
#9280 = VECTOR ( 'NONE', #5836, 1000.000000000000000 ) ;
#9281 = ORIENTED_EDGE ( 'NONE', *, *, #13449, .T. ) ;
#9282 = ADVANCED_FACE ( 'NONE', ( #8637 ), #3347, .T. ) ;
#9283 = DIRECTION ( 'NONE',  ( 0.000000000000000000, 0.000000000000000000, -1.000000000000000000 ) ) ;
#9284 = ORIENTED_EDGE ( 'NONE', *, *, #1407, .T. ) ;
#9285 = ADVANCED_FACE ( 'NONE', ( #6612 ), #10648, .T. ) ;
#9286 = EDGE_LOOP ( 'NONE', ( #7398, #9063 ) ) ;
#9287 = ORIENTED_EDGE ( 'NONE', *, *, #1227, .F. ) ;
#9288 = CARTESIAN_POINT ( 'NONE',  ( -1.059188295049996231, 27.97290950744599769, 58.85000000000000142 ) ) ;
#9289 = VECTOR ( 'NONE', #2119, 1000.000000000000000 ) ;
#9290 = LINE ( 'NONE', #8237, #6713 ) ;
#9291 = DIRECTION ( 'NONE',  ( 1.000000000000000000, 0.000000000000000000, 0.000000000000000000 ) ) ;
#9292 = LINE ( 'NONE', #13540, #6421 ) ;
#9293 = ADVANCED_FACE ( 'NONE', ( #7375 ), #5425, .T. ) ;
#9294 = CARTESIAN_POINT ( 'NONE',  ( -24.10918829505000005, 10.97290950744599947, 14.00000000000000000 ) ) ;
#9295 = FACE_OUTER_BOUND ( 'NONE', #7607, .T. ) ;
#9296 = AXIS2_PLACEMENT_3D ( 'NONE', #1044, #6940, #4077 ) ;
#9297 = ORIENTED_EDGE ( 'NONE', *, *, #10369, .T. ) ;
#9298 = ADVANCED_FACE ( 'NONE', ( #190 ), #4463, .T. ) ;
#9299 = ORIENTED_EDGE ( 'NONE', *, *, #11570, .T. ) ;
#9300 = CARTESIAN_POINT ( 'NONE',  ( -15.05138143747856638, 30.16479851545970092, 54.66128400976000989 ) ) ;
#9301 = EDGE_LOOP ( 'NONE', ( #4666, #3234, #10680, #6727 ) ) ;
#9302 = ORIENTED_EDGE ( 'NONE', *, *, #3377, .T. ) ;
#9303 = CARTESIAN_POINT ( 'NONE',  ( -5.631644894983189431, 10.97290950744599947, 5.250000000000000000 ) ) ;
#9304 = APPLICATION_CONTEXT ( 'automotive_design' ) ;
#9305 = DIRECTION ( 'NONE',  ( 1.000000000000000000, 0.000000000000000000, 0.000000000000000000 ) ) ;
#9306 = ORIENTED_EDGE ( 'NONE', *, *, #9034, .T. ) ;
#9307 = DIRECTION ( 'NONE',  ( 1.000000000000000000, 0.000000000000000000, 0.000000000000000000 ) ) ;
#9308 = CARTESIAN_POINT ( 'NONE',  ( -35.05918829505000645, -6.027090492554000534, 7.250000000000000000 ) ) ;
#9309 = EDGE_CURVE ( 'NONE', #9632, #11638, #11199, .T. ) ;
#9310 = DIRECTION ( 'NONE',  ( 0.7071067811865451302, -0.7071067811865500152, -0.000000000000000000 ) ) ;
#9311 = DIRECTION ( 'NONE',  ( 0.000000000000000000, 0.000000000000000000, -1.000000000000000000 ) ) ;
#9312 = CARTESIAN_POINT ( 'NONE',  ( -19.52085246506412730, 27.91012756408683515, 57.74101035145125849 ) ) ;
#9313 = CARTESIAN_POINT ( 'NONE',  ( 50.63563590245420443, 108.9054980190242503, 22.75000000000000000 ) ) ;
#9314 = VECTOR ( 'NONE', #9976, 1000.000000000000000 ) ;
#9315 = ORIENTED_EDGE ( 'NONE', *, *, #8395, .F. ) ;
#9316 = VERTEX_POINT ( 'NONE', #7432 ) ;
#9317 = CARTESIAN_POINT ( 'NONE',  ( -18.05918829504999934, 10.97290950744599947, 6.250000000000000000 ) ) ;
#9318 = ORIENTED_EDGE ( 'NONE', *, *, #12598, .F. ) ;
#9319 = EDGE_CURVE ( 'NONE', #10483, #5517, #11761, .T. ) ;
#9320 = CARTESIAN_POINT ( 'NONE',  ( -19.47982319660919615, 30.31714196969473463, 61.39763971179084479 ) ) ;
#9321 = AXIS2_PLACEMENT_3D ( 'NONE', #8133, #2852, #6524 ) ;
#9322 = CARTESIAN_POINT ( 'NONE',  ( -25.33503448090910126, 29.19143287883919768, 64.85000000000000853 ) ) ;
#9323 = AXIS2_PLACEMENT_3D ( 'NONE', #13456, #3900, #308 ) ;
#9324 = CARTESIAN_POINT ( 'NONE',  ( -14.95720466168106100, 17.08029827338444662, 64.54999999999999716 ) ) ;
#9325 = DIRECTION ( 'NONE',  ( 0.000000000000000000, 0.000000000000000000, 1.000000000000000000 ) ) ;
#9326 = FACE_BOUND ( 'NONE', #1194, .T. ) ;
#9327 = CARTESIAN_POINT ( 'NONE',  ( 20.44081170494997224, 8.972909507445992361, 163.8499999999999943 ) ) ;
#9328 = ORIENTED_EDGE ( 'NONE', *, *, #9386, .F. ) ;
#9329 = ORIENTED_EDGE ( 'NONE', *, *, #3433, .F. ) ;
#9330 = ORIENTED_EDGE ( 'NONE', *, *, #13261, .F. ) ;
#9331 = AXIS2_PLACEMENT_3D ( 'NONE', #12383, #10156, #12107 ) ;
#9332 = AXIS2_PLACEMENT_3D ( 'NONE', #5601, #232, #2352 ) ;
#9333 = LINE ( 'NONE', #12348, #11289 ) ;
#9334 = LINE ( 'NONE', #4035, #8189 ) ;
#9335 = ORIENTED_EDGE ( 'NONE', *, *, #10369, .F. ) ;
#9336 = DIRECTION ( 'NONE',  ( -0.000000000000000000, -0.000000000000000000, 1.000000000000000000 ) ) ;
#9337 = CYLINDRICAL_SURFACE ( 'NONE', #394, 2.700000000000000178 ) ;
#9338 = CARTESIAN_POINT ( 'NONE',  ( -21.36716865236079954, 14.72221156991656166, 68.84999999999999432 ) ) ;
#9339 = DIRECTION ( 'NONE',  ( 0.000000000000000000, 1.000000000000000000, 0.000000000000000000 ) ) ;
#9340 = CARTESIAN_POINT ( 'NONE',  ( 0.000000000000000000, 4.500000000000000000, 0.000000000000000000 ) ) ;
#9341 = DIRECTION ( 'NONE',  ( 1.000000000000000000, 0.000000000000000000, 0.000000000000000000 ) ) ;
#9342 = DIRECTION ( 'NONE',  ( -0.000000000000000000, -0.000000000000000000, 1.000000000000000000 ) ) ;
#9343 = DIRECTION ( 'NONE',  ( 0.000000000000000000, 1.000000000000000000, 0.000000000000000000 ) ) ;
#9344 = SURFACE_SIDE_STYLE ('',( #9425 ) ) ;
#9345 = AXIS2_PLACEMENT_3D ( 'NONE', #3697, #3843, #6768 ) ;
#9346 = ORIENTED_EDGE ( 'NONE', *, *, #331, .T. ) ;
#9347 = ADVANCED_FACE ( 'NONE', ( #12828 ), #11231, .F. ) ;
#9348 = AXIS2_PLACEMENT_3D ( 'NONE', #4759, #9014, #13268 ) ;
#9349 = AXIS2_PLACEMENT_3D ( 'NONE', #5148, #9423, #6054 ) ;
#9350 = ADVANCED_FACE ( 'NONE', ( #1511 ), #2590, .F. ) ;
#9351 = ADVANCED_FACE ( 'NONE', ( #2458 ), #9532, .T. ) ;
#9352 = PRODUCT_DEFINITION_CONTEXT ( 'detailed design', #7861, 'design' ) ;
#9353 = ORIENTED_EDGE ( 'NONE', *, *, #3213, .T. ) ;
#9354 = EDGE_LOOP ( 'NONE', ( #3657, #13716, #13007, #7528 ) ) ;
#9355 = DIRECTION ( 'NONE',  ( 0.7071067811865451302, -0.7071067811865500152, -0.000000000000000000 ) ) ;
#9356 = AXIS2_PLACEMENT_3D ( 'NONE', #13374, #3890, #10441 ) ;
#9357 = ORIENTED_EDGE ( 'NONE', *, *, #1447, .T. ) ;
#9358 = CARTESIAN_POINT ( 'NONE',  ( -19.30446081463740882, 16.54212282176263926, 68.16277745478451777 ) ) ;
#9359 = LINE ( 'NONE', #10339, #1343 ) ;
#9360 = CIRCLE ( 'NONE', #10702, 6.000000000000002665 ) ;
#9361 = CARTESIAN_POINT ( 'NONE',  ( 42.63563590245419732, 111.0390816101113387, 20.00000000000000000 ) ) ;
#9362 = CIRCLE ( 'NONE', #2018, 0.5000000000000004441 ) ;
#9363 = DIRECTION ( 'NONE',  ( 0.000000000000000000, 0.000000000000000000, 1.000000000000000000 ) ) ;
#9364 = CYLINDRICAL_SURFACE ( 'NONE', #12492, 23.22993838181875148 ) ;
#9365 = EDGE_CURVE ( 'NONE', #3252, #1604, #7931, .T. ) ;
#9366 = EDGE_CURVE ( 'NONE', #13129, #6705, #12205, .T. ) ;
#9367 = CIRCLE ( 'NONE', #13365, 6.000000000000000888 ) ;
#9368 = ORIENTED_EDGE ( 'NONE', *, *, #8487, .F. ) ;
#9369 = EDGE_CURVE ( 'NONE', #13568, #6571, #5767, .T. ) ;
#9370 = CARTESIAN_POINT ( 'NONE',  ( -14.53639149466098957, 30.09164131421196942, 55.64423375431439212 ) ) ;
#9371 = ORIENTED_EDGE ( 'NONE', *, *, #8634, .T. ) ;
#9372 = ORIENTED_EDGE ( 'NONE', *, *, #11243, .T. ) ;
#9373 = ORIENTED_EDGE ( 'NONE', *, *, #497, .F. ) ;
#9374 = FACE_OUTER_BOUND ( 'NONE', #12362, .T. ) ;
#9375 = CARTESIAN_POINT ( 'NONE',  ( -18.05918829504999934, 28.64232754551664684, 57.35000000000000142 ) ) ;
#9376 = ORIENTED_EDGE ( 'NONE', *, *, #1949, .T. ) ;
#9377 = CARTESIAN_POINT ( 'NONE',  ( -10.47404583389237942, 25.90703532196704728, 58.54999999999999716 ) ) ;
#9378 = CARTESIAN_POINT ( 'NONE',  ( -3.125062480528954634, 3.387767046288379991, 61.85000000000000142 ) ) ;
#9379 = ORIENTED_EDGE ( 'NONE', *, *, #400, .T. ) ;
#9380 = CARTESIAN_POINT ( 'NONE',  ( -18.05918829504999934, 10.97290950744599947, 116.8499999999999943 ) ) ;
#9381 = CIRCLE ( 'NONE', #6472, 4.750000000000000888 ) ;
#9382 = AXIS2_PLACEMENT_3D ( 'NONE', #6426, #5372, #6628 ) ;
#9383 = CARTESIAN_POINT ( 'NONE',  ( -40.05918829504999934, -14.02709049255400053, 10.00000000000000000 ) ) ;
#9384 = AXIS2_PLACEMENT_3D ( 'NONE', #11907, #2358, #3527 ) ;
#9385 = CARTESIAN_POINT ( 'NONE',  ( -18.05918829504999934, 10.97290950744599947, 57.35000000000000142 ) ) ;
#9386 = EDGE_CURVE ( 'NONE', #2748, #1420, #3689, .T. ) ;
#9387 = CARTESIAN_POINT ( 'NONE',  ( -39.80918829504999934, 27.97290950744599769, 64.85000000000000853 ) ) ;
#9388 = EDGE_CURVE ( 'NONE', #6784, #6589, #1446, .T. ) ;
#9389 = ORIENTED_EDGE ( 'NONE', *, *, #12363, .F. ) ;
#9390 = ADVANCED_FACE ( 'NONE', ( #2659 ), #13249, .F. ) ;
#9391 = VECTOR ( 'NONE', #13786, 1000.000000000000000 ) ;
#9392 = AXIS2_PLACEMENT_3D ( 'NONE', #5087, #6348, #13608 ) ;
#9393 = AXIS2_PLACEMENT_3D ( 'NONE', #8052, #13293, #11209 ) ;
#9394 = ORIENTED_EDGE ( 'NONE', *, *, #1257, .F. ) ;
#9395 = ORIENTED_EDGE ( 'NONE', *, *, #9198, .F. ) ;
#9396 = ORIENTED_EDGE ( 'NONE', *, *, #2714, .F. ) ;
#9397 = ORIENTED_EDGE ( 'NONE', *, *, #9820, .T. ) ;
#9398 = CARTESIAN_POINT ( 'NONE',  ( -18.05918829504999934, 10.97290950744599947, 0.000000000000000000 ) ) ;
#9399 = DIRECTION ( 'NONE',  ( 0.000000000000000000, -2.202823461557850341E-15, 1.000000000000000000 ) ) ;
#9400 = LINE ( 'NONE', #10435, #2774 ) ;
#9401 = FACE_OUTER_BOUND ( 'NONE', #11951, .T. ) ;
#9402 = LINE ( 'NONE', #1789, #6505 ) ;
#9403 = EDGE_CURVE ( 'NONE', #6080, #5517, #2527, .T. ) ;
#9404 = CARTESIAN_POINT ( 'NONE',  ( 76.11748380738829667, 82.61803701715820125, 19.25000000000000000 ) ) ;
#9405 = AXIS2_PLACEMENT_3D ( 'NONE', #1838, #2831, #13490 ) ;
#9406 = AXIS2_PLACEMENT_3D ( 'NONE', #151, #6582, #5323 ) ;
#9407 = ORIENTED_EDGE ( 'NONE', *, *, #4860, .T. ) ;
#9408 = VECTOR ( 'NONE', #8298, 1000.000000000000000 ) ;
#9409 = VERTEX_POINT ( 'NONE', #11155 ) ;
#9410 = MANIFOLD_SOLID_BREP ( 'NONE', #2812 ) ;
#9411 = EDGE_CURVE ( 'NONE', #2347, #6401, #401, .T. ) ;
#9412 = STYLED_ITEM ( 'NONE', ( #11383 ), #4512 ) ;
#9413 = DIRECTION ( 'NONE',  ( -0.6615960714621564875, 0.7498604124941129490, 0.000000000000000000 ) ) ;
#9414 = AXIS2_PLACEMENT_3D ( 'NONE', #1483, #516, #2630 ) ;
#9415 = ORIENTED_EDGE ( 'NONE', *, *, #1161, .T. ) ;
#9416 = ORIENTED_EDGE ( 'NONE', *, *, #6645, .F. ) ;
#9417 = CARTESIAN_POINT ( 'NONE',  ( -27.49999999999998934, 9.000000000000000000, 29.99999999999999645 ) ) ;
#9418 = CARTESIAN_POINT ( 'NONE',  ( -18.05918829504999934, 10.97290950744599947, 23.90000000000000213 ) ) ;
#9419 = FACE_BOUND ( 'NONE', #3080, .T. ) ;
#9420 = CARTESIAN_POINT ( 'NONE',  ( -7.640422211807256225, -16.89844320975769776, 7.000000000000000000 ) ) ;
#9421 = ORIENTED_EDGE ( 'NONE', *, *, #12814, .F. ) ;
#9422 = FACE_OUTER_BOUND ( 'NONE', #11659, .T. ) ;
#9423 = DIRECTION ( 'NONE',  ( 0.000000000000000000, 0.000000000000000000, 1.000000000000000000 ) ) ;
#9424 = CARTESIAN_POINT ( 'NONE',  ( 140.6356359024541973, 89.90549801902423610, 20.00000000000000000 ) ) ;
#9425 = SURFACE_STYLE_FILL_AREA ( #10390 ) ;
#9426 = EDGE_LOOP ( 'NONE', ( #4633, #4154, #13418, #7143, #12633, #7068 ) ) ;
#9427 = EDGE_LOOP ( 'NONE', ( #2362, #8413, #6046, #6428 ) ) ;
#9428 = ORIENTED_EDGE ( 'NONE', *, *, #10317, .F. ) ;
#9429 = ORIENTED_EDGE ( 'NONE', *, *, #6857, .F. ) ;
#9430 = ADVANCED_BREP_SHAPE_REPRESENTATION ( '', ( #4577, #6434 ), #1075 ) ;
#9431 = CARTESIAN_POINT ( 'NONE',  ( 140.6356359024541973, 113.0390816101113387, 19.25000000000000000 ) ) ;
#9432 = ADVANCED_FACE ( 'NONE', ( #3487 ), #8926, .T. ) ;
#9433 = VERTEX_POINT ( 'NONE', #668 ) ;
#9434 = CARTESIAN_POINT ( 'NONE',  ( -20.26454227913669115, 15.69505033385297921, 68.63899161578964936 ) ) ;
#9435 = CIRCLE ( 'NONE', #4960, 3.800000000000002487 ) ;
#9436 = CARTESIAN_POINT ( 'NONE',  ( -22.64501676333060232, -4.028726038184999858, 62.14999999999999858 ) ) ;
#9437 = EDGE_LOOP ( 'NONE', ( #83, #2110 ) ) ;
#9438 = DIRECTION ( 'NONE',  ( 0.000000000000000000, 0.000000000000000000, 1.000000000000000000 ) ) ;
#9439 = CYLINDRICAL_SURFACE ( 'NONE', #4864, 0.2500000000000002220 ) ;
#9440 = ORIENTED_EDGE ( 'NONE', *, *, #7142, .T. ) ;
#9441 = CARTESIAN_POINT ( 'NONE',  ( -14.50040334037220369, 30.08605482697782918, 58.95214850063695167 ) ) ;
#9442 = ORIENTED_EDGE ( 'NONE', *, *, #12030, .T. ) ;
#9443 = ORIENTED_EDGE ( 'NONE', *, *, #6358, .T. ) ;
#9444 = EDGE_CURVE ( 'NONE', #8730, #4150, #3961, .T. ) ;
#9445 = ORIENTED_EDGE ( 'NONE', *, *, #10856, .T. ) ;
#9446 = DIRECTION ( 'NONE',  ( 0.000000000000000000, 0.000000000000000000, -1.000000000000000000 ) ) ;
#9447 = CARTESIAN_POINT ( 'NONE',  ( 140.6356359024541973, 89.90549801902423610, 22.75000000000000000 ) ) ;
#9448 = ORIENTED_EDGE ( 'NONE', *, *, #4685, .F. ) ;
#9449 = EDGE_CURVE ( 'NONE', #3613, #7821, #1872, .T. ) ;
#9450 = CARTESIAN_POINT ( 'NONE',  ( 140.6356359024541973, 108.9054980190242503, 23.00000000000000000 ) ) ;
#9451 = CARTESIAN_POINT ( 'NONE',  ( -35.05918829505000645, 10.97290950744599947, 63.54999999999999716 ) ) ;
#9452 = EDGE_CURVE ( 'NONE', #9897, #6357, #13664, .T. ) ;
#9453 = CARTESIAN_POINT ( 'NONE',  ( -39.30918829504999934, -6.027090492554000534, 58.85000000000000142 ) ) ;
#9454 = AXIS2_PLACEMENT_3D ( 'NONE', #199, #4084, #12526 ) ;
#9455 = CARTESIAN_POINT ( 'NONE',  ( -19.55918829504999934, 27.90660372932210009, 57.35000000000000142 ) ) ;
#9456 = CARTESIAN_POINT ( 'NONE',  ( 0.000000000000000000, 0.000000000000000000, 7.000000000000000000 ) ) ;
#9457 = AXIS2_PLACEMENT_3D ( 'NONE', #3907, #2946, #751 ) ;
#9458 = VERTEX_POINT ( 'NONE', #5139 ) ;
#9459 = EDGE_CURVE ( 'NONE', #5647, #12210, #5496, .T. ) ;
#9460 = ORIENTED_EDGE ( 'NONE', *, *, #12563, .T. ) ;
#9461 = EDGE_LOOP ( 'NONE', ( #6847, #8058, #3052, #7664 ) ) ;
#9462 = VERTEX_POINT ( 'NONE', #1721 ) ;
#9463 = DIRECTION ( 'NONE',  ( -0.000000000000000000, 1.000000000000000000, -0.000000000000000000 ) ) ;
#9464 = CARTESIAN_POINT ( 'NONE',  ( 112.1804561881462945, 85.03908161011133870, 0.7500000000000006661 ) ) ;
#9465 = CARTESIAN_POINT ( 'NONE',  ( -20.04118352984052720, 30.27579076659624135, 61.07633196088716687 ) ) ;
#9466 = CARTESIAN_POINT ( 'NONE',  ( -35.05918829505000645, 27.97290950744599769, 64.85000000000000853 ) ) ;
#9467 = DIRECTION ( 'NONE',  ( -1.000000000000000000, -0.000000000000000000, -0.000000000000000000 ) ) ;
#9468 = CARTESIAN_POINT ( 'NONE',  ( -4.599650328638321461, 8.500000000000000000, -7.878124499050794149 ) ) ;
#9469 = EDGE_CURVE ( 'NONE', #10379, #1230, #12480, .T. ) ;
#9470 = DIRECTION ( 'NONE',  ( -1.000000000000000000, 0.000000000000000000, 0.000000000000000000 ) ) ;
#9471 = VERTEX_POINT ( 'NONE', #7221 ) ;
#9472 = EDGE_CURVE ( 'NONE', #8191, #10469, #10530, .T. ) ;
#9473 = ORIENTED_EDGE ( 'NONE', *, *, #7998, .T. ) ;
#9474 = DIRECTION ( 'NONE',  ( 1.000000000000000000, 0.000000000000000000, 0.000000000000000000 ) ) ;
#9475 = FACE_OUTER_BOUND ( 'NONE', #9223, .T. ) ;
#9476 = ORIENTED_EDGE ( 'NONE', *, *, #754, .T. ) ;
#9477 = LINE ( 'NONE', #7420, #5584 ) ;
#9478 = LINE ( 'NONE', #13722, #3530 ) ;
#9479 = FACE_OUTER_BOUND ( 'NONE', #12021, .T. ) ;
#9480 = FACE_OUTER_BOUND ( 'NONE', #10273, .T. ) ;
#9481 = ORIENTED_EDGE ( 'NONE', *, *, #8831, .T. ) ;
#9482 = CARTESIAN_POINT ( 'NONE',  ( -11.74835982676941981, -4.028726038184999858, 62.14999999999999858 ) ) ;
#9483 = DIRECTION ( 'NONE',  ( 1.000000000000000000, 0.000000000000000000, 0.000000000000000000 ) ) ;
#9484 = DIRECTION ( 'NONE',  ( 1.000000000000000000, 0.000000000000000000, 0.000000000000000000 ) ) ;
#9485 = EDGE_CURVE ( 'NONE', #8835, #12176, #881, .T. ) ;
#9486 = CARTESIAN_POINT ( 'NONE',  ( 140.6356359024541973, 89.90549801902423610, 22.75000000000000000 ) ) ;
#9487 = DIRECTION ( 'NONE',  ( 0.000000000000000000, 0.000000000000000000, 1.000000000000000000 ) ) ;
#9488 = CLOSED_SHELL ( 'NONE', ( #12668, #2580, #4751, #5430, #11208, #9105, #5710, #9769, #6383, #4087, #8046, #8172, #11815, #2148, #1582, #3327, #4573, #492 ) ) ;
#9489 = EDGE_LOOP ( 'NONE', ( #637, #9765, #5085, #5589 ) ) ;
#9490 = DIRECTION ( 'NONE',  ( -0.000000000000000000, -1.000000000000000000, 0.000000000000000000 ) ) ;
#9491 = VERTEX_POINT ( 'NONE', #958 ) ;
#9492 = DIRECTION ( 'NONE',  ( 0.000000000000000000, 0.000000000000000000, -1.000000000000000000 ) ) ;
#9493 = VERTEX_POINT ( 'NONE', #13384 ) ;
#9494 = CARTESIAN_POINT ( 'NONE',  ( 116.7775623211734342, 85.78908161011133870, 0.7500000000000000000 ) ) ;
#9495 = CARTESIAN_POINT ( 'NONE',  ( -30.30918829504999934, -6.027090492554000534, 7.250000000000000000 ) ) ;
#9496 = CARTESIAN_POINT ( 'NONE',  ( -14.96009381531125015, 7.039309042655558457, 68.84999999999999432 ) ) ;
#9497 = AXIS2_PLACEMENT_3D ( 'NONE', #10136, #5783, #12013 ) ;
#9498 = CARTESIAN_POINT ( 'NONE',  ( -28.87730642030695094, -7.867426463707980488, 5.250000000000000000 ) ) ;
#9499 = EDGE_CURVE ( 'NONE', #4952, #11290, #9754, .T. ) ;
#9500 = VECTOR ( 'NONE', #3828, 1000.000000000000000 ) ;
#9501 = CARTESIAN_POINT ( 'NONE',  ( -15.29370303376928852, 30.19507513566514234, 60.35551381422868644 ) ) ;
#9502 = ORIENTED_EDGE ( 'NONE', *, *, #12632, .T. ) ;
#9503 = ORIENTED_EDGE ( 'NONE', *, *, #4447, .T. ) ;
#9504 = ORIENTED_EDGE ( 'NONE', *, *, #3739, .T. ) ;
#9505 = ORIENTED_EDGE ( 'NONE', *, *, #11455, .T. ) ;
#9506 = CARTESIAN_POINT ( 'NONE',  ( 50.63563590245420443, 89.90549801902423610, 22.75000000000000000 ) ) ;
#9507 = DIRECTION ( 'NONE',  ( -1.000000000000000000, 0.000000000000000000, 0.000000000000000000 ) ) ;
#9508 = FACE_OUTER_BOUND ( 'NONE', #11689, .T. ) ;
#9509 = CARTESIAN_POINT ( 'NONE',  ( -19.71317847370539766, 12.84756053868127879, 67.84999999999999432 ) ) ;
#9510 = FACE_OUTER_BOUND ( 'NONE', #3481, .T. ) ;
#9511 = CARTESIAN_POINT ( 'NONE',  ( -18.05918829504999223, 2.756898754446003963, 63.36264408500002787 ) ) ;
#9512 = VECTOR ( 'NONE', #11677, 999.9999999999998863 ) ;
#9513 = CARTESIAN_POINT ( 'NONE',  ( -9.759188295050000406, 10.97290950744599947, 61.86500000000000199 ) ) ;
#9514 = ADVANCED_FACE ( 'NONE', ( #806 ), #5208, .F. ) ;
#9515 = EDGE_CURVE ( 'NONE', #4114, #3872, #2024, .T. ) ;
#9516 = EDGE_LOOP ( 'NONE', ( #775, #7234 ) ) ;
#9517 = VERTEX_POINT ( 'NONE', #2800 ) ;
#9518 =( BOUNDED_CURVE ( )  B_SPLINE_CURVE ( 3, ( #6907, #8950, #2815, #13205 ),
 .UNSPECIFIED., .F., .F. ) 
 B_SPLINE_CURVE_WITH_KNOTS ( ( 4, 4 ),
 ( 4.712388980384689674, 6.283185307179586232 ),
 .UNSPECIFIED. ) 
 CURVE ( )  GEOMETRIC_REPRESENTATION_ITEM ( )  RATIONAL_B_SPLINE_CURVE ( ( 1.000000000000000000, 0.8047378541243649375, 0.8047378541243649375, 1.000000000000000000 ) ) 
 REPRESENTATION_ITEM ( '' )  );
#9519 = ORIENTED_EDGE ( 'NONE', *, *, #8938, .T. ) ;
#9520 = ORIENTED_EDGE ( 'NONE', *, *, #12696, .F. ) ;
#9521 = ORIENTED_EDGE ( 'NONE', *, *, #11013, .T. ) ;
#9522 = DIRECTION ( 'NONE',  ( 1.000000000000000000, -0.000000000000000000, -0.000000000000000000 ) ) ;
#9523 = CARTESIAN_POINT ( 'NONE',  ( 42.94629607423402007, 87.16776126655173584, 20.00000000000000000 ) ) ;
#9524 = PLANE ( 'NONE',  #12310 ) ;
#9525 = CARTESIAN_POINT ( 'NONE',  ( -19.47340185742309870, 26.91028695795525039, 56.84999999999999432 ) ) ;
#9526 = DIRECTION ( 'NONE',  ( 0.000000000000000000, 0.000000000000000000, 1.000000000000000000 ) ) ;
#9527 = CARTESIAN_POINT ( 'NONE',  ( -18.05918829504999934, 10.97290950744599947, 62.14999999999999858 ) ) ;
#9528 = CARTESIAN_POINT ( 'NONE',  ( 116.7775623211734342, 75.03908161011133870, 20.00000000000000000 ) ) ;
#9529 = CONTEXT_DEPENDENT_SHAPE_REPRESENTATION ( #6167, #13056 ) ;
#9530 = ORIENTED_EDGE ( 'NONE', *, *, #12612, .T. ) ;
#9531 = EDGE_CURVE ( 'NONE', #1997, #4071, #5068, .T. ) ;
#9532 = CONICAL_SURFACE ( 'NONE', #5280, 2.800000000000000266, 0.7853981633974419507 ) ;
#9533 = EDGE_CURVE ( 'NONE', #1281, #11638, #10877, .T. ) ;
#9534 = VERTEX_POINT ( 'NONE', #8293 ) ;
#9535 = FACE_OUTER_BOUND ( 'NONE', #5515, .T. ) ;
#9536 = ADVANCED_FACE ( 'NONE', ( #11366 ), #10211, .T. ) ;
#9537 = ORIENTED_EDGE ( 'NONE', *, *, #5245, .F. ) ;
#9538 = CIRCLE ( 'NONE', #10434, 6.049999999999999822 ) ;
#9539 = CARTESIAN_POINT ( 'NONE',  ( 50.38563590245420443, 90.15549801902423610, 23.00000000000000000 ) ) ;
#9540 = VECTOR ( 'NONE', #7165, 1000.000000000000000 ) ;
#9541 = LINE ( 'NONE', #12618, #6934 ) ;
#9542 = CARTESIAN_POINT ( 'NONE',  ( 50.38563590245420443, 108.6554980190242503, 23.00000000000000000 ) ) ;
#9543 = CIRCLE ( 'NONE', #2873, 6.000000000000002665 ) ;
#9544 = DIRECTION ( 'NONE',  ( 0.4528443260392608360, 0.8915896008669278450, 0.000000000000000000 ) ) ;
#9545 = EDGE_LOOP ( 'NONE', ( #6578, #10509, #9902, #3067 ) ) ;
#9546 = FACE_OUTER_BOUND ( 'NONE', #11126, .T. ) ;
#9547 = CARTESIAN_POINT ( 'NONE',  ( 142.6356359024541973, 87.03908161011133870, 19.68933982822018081 ) ) ;
#9548 = DIRECTION ( 'NONE',  ( 0.000000000000000000, 0.000000000000000000, -1.000000000000000000 ) ) ;
#9549 = FACE_BOUND ( 'NONE', #1034, .T. ) ;
#9550 = VERTEX_POINT ( 'NONE', #5003 ) ;
#9551 = ADVANCED_FACE ( 'NONE', ( #9271 ), #9337, .F. ) ;
#9552 = AXIS2_PLACEMENT_3D ( 'NONE', #10478, #11670, #6205 ) ;
#9553 = AXIS2_PLACEMENT_3D ( 'NONE', #8145, #9463, #8008 ) ;
#9554 = AXIS2_PLACEMENT_3D ( 'NONE', #4962, #10340, #6202 ) ;
#9555 = AXIS2_PLACEMENT_3D ( 'NONE', #1785, #4852, #13368 ) ;
#9556 = VERTEX_POINT ( 'NONE', #8215 ) ;
#9557 = EDGE_CURVE ( 'NONE', #5483, #5782, #11988, .T. ) ;
#9558 = DIRECTION ( 'NONE',  ( 1.000000000000000000, 0.000000000000000000, 0.000000000000000000 ) ) ;
#9559 = CARTESIAN_POINT ( 'NONE',  ( -13.45272330285627582, 8.369250445964327767, 68.55863802020633102 ) ) ;
#9560 = DIRECTION ( 'NONE',  ( 0.000000000000000000, 0.000000000000000000, -1.000000000000000000 ) ) ;
#9561 = PRESENTATION_LAYER_ASSIGNMENT (  '', '', ( #9796 ) ) ;
#9562 = DIRECTION ( 'NONE',  ( -1.000000000000000000, 0.000000000000000000, 0.000000000000000000 ) ) ;
#9563 = AXIS2_PLACEMENT_3D ( 'NONE', #992, #1983, #9307 ) ;
#9564 = CIRCLE ( 'NONE', #4891, 0.9499999999999995115 ) ;
#9565 = CARTESIAN_POINT ( 'NONE',  ( -15.27817205863298256, 6.758671056314481618, 68.81396957244685098 ) ) ;
#9566 = VECTOR ( 'NONE', #1593, 1000.000000000000000 ) ;
#9567 = DIRECTION ( 'NONE',  ( -1.000000000000000000, 0.000000000000000000, 0.000000000000000000 ) ) ;
#9568 = APPLICATION_CONTEXT ( 'automotive_design' ) ;
#9569 = AXIS2_PLACEMENT_3D ( 'NONE', #3548, #2516, #1578 ) ;
#9570 = AXIS2_PLACEMENT_3D ( 'NONE', #12227, #358, #7813 ) ;
#9571 = EDGE_CURVE ( 'NONE', #10203, #1958, #8876, .T. ) ;
#9572 = DIRECTION ( 'NONE',  ( -1.182766006347823109E-16, 1.000000000000000000, -0.000000000000000000 ) ) ;
#9573 = ORIENTED_EDGE ( 'NONE', *, *, #12093, .F. ) ;
#9574 = ORIENTED_EDGE ( 'NONE', *, *, #296, .T. ) ;
#9575 = DIRECTION ( 'NONE',  ( 0.000000000000000000, 0.000000000000000000, -1.000000000000000000 ) ) ;
#9576 = CARTESIAN_POINT ( 'NONE',  ( 141.8856359024541973, 110.7284214383315089, 20.00000000000000000 ) ) ;
#9577 = CARTESIAN_POINT ( 'NONE',  ( -18.05918829504999934, 10.97290950744599947, 7.250000000000000000 ) ) ;
#9578 = CARTESIAN_POINT ( 'NONE',  ( 1.653273178848926867E-15, 4.500000000000000000, 13.50000000000000000 ) ) ;
#9579 = DIRECTION ( 'NONE',  ( 0.000000000000000000, 0.000000000000000000, 1.000000000000000000 ) ) ;
#9580 = LINE ( 'NONE', #12661, #7805 ) ;
#9581 = VECTOR ( 'NONE', #2497, 1000.000000000000000 ) ;
#9582 = VECTOR ( 'NONE', #4249, 1000.000000000000114 ) ;
#9583 = ORIENTED_EDGE ( 'NONE', *, *, #5217, .F. ) ;
#9584 = VERTEX_POINT ( 'NONE', #11647 ) ;
#9585 = ORIENTED_EDGE ( 'NONE', *, *, #13776, .T. ) ;
#9586 = DIRECTION ( 'NONE',  ( -0.3132098788326386218, -0.9496839325805422893, 0.000000000000000000 ) ) ;
#9587 = VERTEX_POINT ( 'NONE', #4314 ) ;
#9588 = VERTEX_POINT ( 'NONE', #6391 ) ;
#9589 = ORIENTED_EDGE ( 'NONE', *, *, #8562, .F. ) ;
#9590 = AXIS2_PLACEMENT_3D ( 'NONE', #7769, #8823, #240 ) ;
#9591 = ADVANCED_FACE ( 'NONE', ( #2369 ), #6464, .T. ) ;
#9592 = ORIENTED_EDGE ( 'NONE', *, *, #2992, .T. ) ;
#9593 = LINE ( 'NONE', #24, #7306 ) ;
#9594 = EDGE_CURVE ( 'NONE', #7101, #10854, #11114, .T. ) ;
#9595 = DIRECTION ( 'NONE',  ( 1.000000000000000000, 0.000000000000000000, 0.000000000000000000 ) ) ;
#9596 = ORIENTED_EDGE ( 'NONE', *, *, #9124, .F. ) ;
#9597 = LINE ( 'NONE', #2354, #1368 ) ;
#9598 = CARTESIAN_POINT ( 'NONE',  ( -24.80918829504999934, 10.97290950744599947, 63.35000000000000142 ) ) ;
#9599 = EDGE_CURVE ( 'NONE', #4496, #12910, #9543, .T. ) ;
#9600 = DIRECTION ( 'NONE',  ( 0.000000000000000000, 0.000000000000000000, -1.000000000000000000 ) ) ;
#9601 = DIRECTION ( 'NONE',  ( 1.000000000000000000, 0.000000000000000000, 0.000000000000000000 ) ) ;
#9602 = FACE_OUTER_BOUND ( 'NONE', #895, .T. ) ;
#9603 = ITEM_DEFINED_TRANSFORMATION ( 'NONE', 'NONE', #9356,  #6434 ) ;
#9604 = ORIENTED_EDGE ( 'NONE', *, *, #8769, .F. ) ;
#9605 = AXIS2_PLACEMENT_3D ( 'NONE', #13248, #12203, #6550 ) ;
#9606 = CIRCLE ( 'NONE', #4042, 4.250000000000000000 ) ;
#9607 = VECTOR ( 'NONE', #9310, 1000.000000000000114 ) ;
#9608 = ORIENTED_EDGE ( 'NONE', *, *, #12434, .F. ) ;
#9609 = LINE ( 'NONE', #10727, #12629 ) ;
#9610 = LINE ( 'NONE', #3329, #5495 ) ;
#9611 = DIRECTION ( 'NONE',  ( -1.000000000000000000, 0.000000000000000000, 0.000000000000000000 ) ) ;
#9612 = EDGE_CURVE ( 'NONE', #5932, #13749, #1779, .T. ) ;
#9613 =( LENGTH_UNIT ( ) NAMED_UNIT ( * ) SI_UNIT ( .MILLI., .METRE. ) );
#9614 = CARTESIAN_POINT ( 'NONE',  ( -19.98782365351838664, 30.28009008643348210, 53.58950411947810721 ) ) ;
#9615 = VECTOR ( 'NONE', #4078, 1000.000000000000000 ) ;
#9616 = VECTOR ( 'NONE', #12001, 1000.000000000000000 ) ;
#9617 = VERTEX_POINT ( 'NONE', #11918 ) ;
#9618 = DIRECTION ( 'NONE',  ( 1.000000000000000000, 0.000000000000000000, 0.000000000000000000 ) ) ;
#9619 = EDGE_LOOP ( 'NONE', ( #11658, #7580, #10865, #1245 ) ) ;
#9620 = DIRECTION ( 'NONE',  ( 0.000000000000000000, 0.000000000000000000, 1.000000000000000000 ) ) ;
#9621 = AXIS2_PLACEMENT_3D ( 'NONE', #8701, #11775, #1158 ) ;
#9622 = EDGE_CURVE ( 'NONE', #8225, #12769, #9685, .T. ) ;
#9623 = DIRECTION ( 'NONE',  ( -0.000000000000000000, -0.000000000000000000, 1.000000000000000000 ) ) ;
#9624 = CARTESIAN_POINT ( 'NONE',  ( -26.35918829505000005, 10.97290950744599947, 63.14999999999999858 ) ) ;
#9625 = ORIENTED_EDGE ( 'NONE', *, *, #7691, .F. ) ;
#9626 = CARTESIAN_POINT ( 'NONE',  ( 111.0903281124166710, 100.8715034839261762, 20.00000000000000000 ) ) ;
#9627 = PRODUCT_DEFINITION ( 'UNKNOWN', '', #12025, #681 ) ;
#9628 = ADVANCED_FACE ( 'NONE', ( #5409 ), #6595, .T. ) ;
#9629 = VECTOR ( 'NONE', #8525, 1000.000000000000000 ) ;
#9630 = CIRCLE ( 'NONE', #4727, 6.299999999999998046 ) ;
#9631 = CIRCLE ( 'NONE', #5375, 16.75000000000000355 ) ;
#9632 = VERTEX_POINT ( 'NONE', #12817 ) ;
#9633 = CARTESIAN_POINT ( 'NONE',  ( -35.05918829505000645, 27.97290950744599769, 10.00000000000000000 ) ) ;
#9634 = ORIENTED_EDGE ( 'NONE', *, *, #10096, .F. ) ;
#9635 = MANIFOLD_SOLID_BREP ( 'Mirror1', #8371 ) ;
#9636 = ORIENTED_EDGE ( 'NONE', *, *, #8285, .F. ) ;
#9638 = EDGE_CURVE ( 'NONE', #12422, #2347, #8202, .T. ) ;
#9637 = ORIENTED_EDGE ( 'NONE', *, *, #11492, .F. ) ;
#9639 = DIRECTION ( 'NONE',  ( 1.000000000000000000, 0.000000000000000000, -0.000000000000000000 ) ) ;
#9640 = DIRECTION ( 'NONE',  ( 1.000000000000000000, 0.000000000000000000, 0.000000000000000000 ) ) ;
#9641 = FACE_OUTER_BOUND ( 'NONE', #1078, .T. ) ;
#9642 = AXIS2_PLACEMENT_3D ( 'NONE', #1450, #10976, #6616 ) ;
#9643 = CARTESIAN_POINT ( 'NONE',  ( -10.38347696868452097, 26.08535324214045303, 57.54999999999999716 ) ) ;
#9644 = DIRECTION ( 'NONE',  ( -0.000000000000000000, -0.000000000000000000, -1.000000000000000000 ) ) ;
#9645 = EDGE_CURVE ( 'NONE', #3675, #10778, #9478, .T. ) ;
#9646 = AXIS2_PLACEMENT_3D ( 'NONE', #7358, #1154, #11650 ) ;
#9647 = DIRECTION ( 'NONE',  ( 1.000000000000000000, 0.000000000000000000, 0.000000000000000000 ) ) ;
#9648 = ORIENTED_EDGE ( 'NONE', *, *, #828, .F. ) ;
#9649 = VERTEX_POINT ( 'NONE', #8420 ) ;
#9650 = ORIENTED_EDGE ( 'NONE', *, *, #662, .T. ) ;
#9651 = EDGE_CURVE ( 'NONE', #2296, #5838, #12442, .T. ) ;
#9652 = CARTESIAN_POINT ( 'NONE',  ( 76.18094369249178044, 97.20665973629650125, 10.00000000000000000 ) ) ;
#9653 = CARTESIAN_POINT ( 'NONE',  ( -1.059188295049996231, 27.97290950744599769, 5.250000000000000000 ) ) ;
#9654 = CARTESIAN_POINT ( 'NONE',  ( -22.95314638948480379, -5.307421391215619622, 62.14999999999999858 ) ) ;
#9655 = FACE_OUTER_BOUND ( 'NONE', #3452, .T. ) ;
#9656 = FACE_OUTER_BOUND ( 'NONE', #304, .T. ) ;
#9657 = EDGE_CURVE ( 'NONE', #4563, #707, #4859, .T. ) ;
#9658 = DIRECTION ( 'NONE',  ( -1.000000000000000000, 0.000000000000000000, 0.000000000000000000 ) ) ;
#9659 = CIRCLE ( 'NONE', #7396, 0.5000000000000004441 ) ;
#9660 = PRODUCT ( 'Base Mounting Plate', 'Base Mounting Plate', '', ( #4930 ) ) ;
#9661 = EDGE_LOOP ( 'NONE', ( #12648, #10636, #10204, #8969, #13220, #4847, #12930, #3291, #2280 ) ) ;
#9662 = ORIENTED_EDGE ( 'NONE', *, *, #5380, .T. ) ;
#9663 = CARTESIAN_POINT ( 'NONE',  ( -4.059188295049996675, 27.97290950744599769, 10.00000000000000000 ) ) ;
#9664 = ORIENTED_EDGE ( 'NONE', *, *, #3168, .F. ) ;
#9665 = VERTEX_POINT ( 'NONE', #8555 ) ;
#9666 = ORIENTED_EDGE ( 'NONE', *, *, #5011, .F. ) ;
#9667 = CIRCLE ( 'NONE', #11447, 1.999999999999994893 ) ;
#9668 = ORIENTED_EDGE ( 'NONE', *, *, #9386, .T. ) ;
#9669 = CARTESIAN_POINT ( 'NONE',  ( 0.000000000000000000, 108.6554980190242503, 22.75000000000000000 ) ) ;
#9670 = CARTESIAN_POINT ( 'NONE',  ( 2.877919977996279531E-15, 4.500000000000000000, 23.49999999999999645 ) ) ;
#9671 = EDGE_LOOP ( 'NONE', ( #7373, #9252, #987, #5433 ) ) ;
#9672 = FACE_BOUND ( 'NONE', #13402, .T. ) ;
#9673 = DIRECTION ( 'NONE',  ( 0.000000000000000000, 1.000000000000000000, 0.000000000000000000 ) ) ;
#9674 = DIRECTION ( 'NONE',  ( 1.000000000000000000, 0.000000000000000000, 0.000000000000000000 ) ) ;
#9675 = DIRECTION ( 'NONE',  ( 0.4528443260392607250, 0.8915896008669278450, 0.000000000000000000 ) ) ;
#9676 = DIRECTION ( 'NONE',  ( 0.000000000000000000, 0.000000000000000000, 1.000000000000000000 ) ) ;
#9677 = PRODUCT_CONTEXT ( 'NONE', #8137, 'mechanical' ) ;
#9678 = VECTOR ( 'NONE', #12834, 1000.000000000000000 ) ;
#9679 = EDGE_CURVE ( 'NONE', #2014, #4651, #3269, .T. ) ;
#9680 = ORIENTED_EDGE ( 'NONE', *, *, #315, .F. ) ;
#9681 = DIRECTION ( 'NONE',  ( -0.000000000000000000, -0.000000000000000000, 1.000000000000000000 ) ) ;
#9682 = EDGE_LOOP ( 'NONE', ( #1293, #12393 ) ) ;
#9683 = DIRECTION ( 'NONE',  ( 0.000000000000000000, 0.000000000000000000, 1.000000000000000000 ) ) ;
#9684 = DIRECTION ( 'NONE',  ( 0.000000000000000000, 0.000000000000000000, 1.000000000000000000 ) ) ;
#9685 = LINE ( 'NONE', #3138, #9086 ) ;
#9686 = CARTESIAN_POINT ( 'NONE',  ( -20.51890800742826571, 30.22967062585348685, 54.01748261881041913 ) ) ;
#9687 = DIRECTION ( 'NONE',  ( 0.000000000000000000, 0.000000000000000000, -1.000000000000000000 ) ) ;
#9688 = ORIENTED_EDGE ( 'NONE', *, *, #11038, .T. ) ;
#9689 = DIRECTION ( 'NONE',  ( 1.000000000000000000, 0.000000000000000000, 0.000000000000000000 ) ) ;
#9690 = CARTESIAN_POINT ( 'NONE',  ( 142.3249757306743675, 87.16776126655166479, 20.00000000000000000 ) ) ;
#9691 = DIRECTION ( 'NONE',  ( 0.6615960714621572647, -0.7498604124941123938, 0.000000000000000000 ) ) ;
#9692 = CARTESIAN_POINT ( 'NONE',  ( -3.999999999999997335, 2.000000000000000000, -65.00000000000000000 ) ) ;
#9693 =( BOUNDED_CURVE ( )  B_SPLINE_CURVE ( 3, ( #2541, #8865, #4812, #13259 ),
 .UNSPECIFIED., .F., .F. ) 
 B_SPLINE_CURVE_WITH_KNOTS ( ( 4, 4 ),
 ( 3.141592653589792672, 4.712388980384689674 ),
 .UNSPECIFIED. ) 
 CURVE ( )  GEOMETRIC_REPRESENTATION_ITEM ( )  RATIONAL_B_SPLINE_CURVE ( ( 1.000000000000000000, 0.8047378541243649375, 0.8047378541243649375, 1.000000000000000000 ) ) 
 REPRESENTATION_ITEM ( '' )  );
#9694 = EDGE_CURVE ( 'NONE', #878, #12860, #5955, .T. ) ;
#9695 = ORIENTED_EDGE ( 'NONE', *, *, #9015, .F. ) ;
#9696 = ORIENTED_EDGE ( 'NONE', *, *, #10071, .T. ) ;
#9697 = CARTESIAN_POINT ( 'NONE',  ( -30.80918829504999934, 27.97290950744599769, 64.85000000000000853 ) ) ;
#9698 = ORIENTED_EDGE ( 'NONE', *, *, #7658, .T. ) ;
#9699 = ORIENTED_EDGE ( 'NONE', *, *, #10649, .T. ) ;
#9700 = DIRECTION ( 'NONE',  ( -1.000000000000000000, 0.000000000000000000, 0.000000000000000000 ) ) ;
#9701 = CARTESIAN_POINT ( 'NONE',  ( 2.262399129208279902, 22.44393519180574970, 17.25000000000000000 ) ) ;
#9702 = CARTESIAN_POINT ( 'NONE',  ( -11.38420496205000099, 17.64789284044599782, 60.40999999999999659 ) ) ;
#9703 = ORIENTED_EDGE ( 'NONE', *, *, #1167, .F. ) ;
#9704 = DIRECTION ( 'NONE',  ( 0.000000000000000000, 0.000000000000000000, -1.000000000000000000 ) ) ;
#9705 = CARTESIAN_POINT ( 'NONE',  ( -18.05918829504999934, 10.97290950744599947, 5.250000000000000000 ) ) ;
#9706 = FACE_OUTER_BOUND ( 'NONE', #4533, .T. ) ;
#9707 = LINE ( 'NONE', #10687, #1990 ) ;
#9708 = CONICAL_SURFACE ( 'NONE', #7230, 4.250000000000000000, 0.7853981633974518317 ) ;
#9709 = EDGE_CURVE ( 'NONE', #5576, #7736, #10220, .T. ) ;
#9710 = VERTEX_POINT ( 'NONE', #9898 ) ;
#9711 = CARTESIAN_POINT ( 'NONE',  ( -15.83529908340206305, 30.25357667928068750, 53.80883379359870133 ) ) ;
#9712 = ORIENTED_EDGE ( 'NONE', *, *, #5706, .F. ) ;
#9713 = DIRECTION ( 'NONE',  ( 0.000000000000000000, 1.000000000000000000, 0.000000000000000000 ) ) ;
#9714 = EDGE_CURVE ( 'NONE', #2711, #6329, #1494, .T. ) ;
#9715 = CIRCLE ( 'NONE', #361, 3.000000000000002665 ) ;
#9716 = CARTESIAN_POINT ( 'NONE',  ( -12.00000000000000000, 2.500000000000000000, -65.00000000000000000 ) ) ;
#9717 = CARTESIAN_POINT ( 'NONE',  ( 6.000000000000000888, 0.000000000000000000, -43.00000000000000000 ) ) ;
#9718 = DIRECTION ( 'NONE',  ( -0.000000000000000000, -0.000000000000000000, 1.000000000000000000 ) ) ;
#9719 = DIRECTION ( 'NONE',  ( 0.000000000000000000, 0.000000000000000000, 1.000000000000000000 ) ) ;
#9720 = FACE_OUTER_BOUND ( 'NONE', #4844, .T. ) ;
#9721 = FACE_OUTER_BOUND ( 'NONE', #12601, .T. ) ;
#9722 = EDGE_CURVE ( 'NONE', #6494, #4217, #6177, .T. ) ;
#9723 = AXIS2_PLACEMENT_3D ( 'NONE', #11363, #877, #2933 ) ;
#9724 = ORIENTED_EDGE ( 'NONE', *, *, #2823, .F. ) ;
#9725 = CARTESIAN_POINT ( 'NONE',  ( -18.05918829504999934, 2.872909508741170015, 63.35000000000700027 ) ) ;
#9726 = ORIENTED_EDGE ( 'NONE', *, *, #7067, .F. ) ;
#9727 = ORIENTED_EDGE ( 'NONE', *, *, #13635, .T. ) ;
#9728 = ORIENTED_EDGE ( 'NONE', *, *, #7822, .F. ) ;
#9729 = ADVANCED_FACE ( 'NONE', ( #11141 ), #9040, .T. ) ;
#9730 = DIRECTION ( 'NONE',  ( -0.000000000000000000, -0.000000000000000000, -1.000000000000000000 ) ) ;
#9731 = LINE ( 'NONE', #13768, #3318 ) ;
#9732 = ORIENTED_EDGE ( 'NONE', *, *, #5793, .T. ) ;
#9733 = CIRCLE ( 'NONE', #2615, 6.049999999999999822 ) ;
#9734 = CARTESIAN_POINT ( 'NONE',  ( -36.55918829504999934, 10.97290950744599947, 14.00000000000000000 ) ) ;
#9735 = FACE_OUTER_BOUND ( 'NONE', #4691, .T. ) ;
#9736 = CARTESIAN_POINT ( 'NONE',  ( -18.05918829504999934, 19.05294282444599929, 63.34900083300000517 ) ) ;
#9737 = DIRECTION ( 'NONE',  ( 0.000000000000000000, 0.000000000000000000, -1.000000000000000000 ) ) ;
#9738 = DIRECTION ( 'NONE',  ( 0.000000000000000000, 0.000000000000000000, -1.000000000000000000 ) ) ;
#9739 = AXIS2_PLACEMENT_3D ( 'NONE', #10400, #5223, #823 ) ;
#9740 = ORIENTED_EDGE ( 'NONE', *, *, #2965, .F. ) ;
#9741 = EDGE_LOOP ( 'NONE', ( #13656, #267, #10635, #2489 ) ) ;
#9742 = EDGE_CURVE ( 'NONE', #10095, #8747, #323, .T. ) ;
#9743 = CARTESIAN_POINT ( 'NONE',  ( -18.05918829504999934, 10.97290950744599947, 0.000000000000000000 ) ) ;
#9744 = CARTESIAN_POINT ( 'NONE',  ( 84.99521369064696330, 82.14063840035363739, 10.00000000000000000 ) ) ;
#9745 = CARTESIAN_POINT ( 'NONE',  ( 68.49370948373500312, 85.78908161011133870, 19.25000000000000000 ) ) ;
#9746 = SURFACE_STYLE_FILL_AREA ( #8489 ) ;
#9747 = CARTESIAN_POINT ( 'NONE',  ( -20.26821253650571464, 30.25500104533646706, 53.79675021559635439 ) ) ;
#9749 = DIRECTION ( 'NONE',  ( 0.000000000000000000, 0.000000000000000000, 1.000000000000000000 ) ) ;
#9748 = APPLICATION_CONTEXT ( 'automotive_design' ) ;
#9750 = AXIS2_PLACEMENT_3D ( 'NONE', #5136, #2934, #11569 ) ;
#9751 = CARTESIAN_POINT ( 'NONE',  ( -18.05918829504999934, 18.59295644444599915, 61.63595870800000398 ) ) ;
#9752 = DIRECTION ( 'NONE',  ( 0.000000000000000000, 0.000000000000000000, 1.000000000000000000 ) ) ;
#9753 = DIRECTION ( 'NONE',  ( 0.000000000000000000, 0.000000000000000000, 1.000000000000000000 ) ) ;
#9754 = CIRCLE ( 'NONE', #6841, 17.00000000000000355 ) ;
#9755 = DIRECTION ( 'NONE',  ( -0.2878798879079283446, 0.9576665234506834823, 0.000000000000000000 ) ) ;
#9756 = CIRCLE ( 'NONE', #13760, 2.000000000000001776 ) ;
#9757 = ORIENTED_EDGE ( 'NONE', *, *, #3592, .F. ) ;
#9758 = CIRCLE ( 'NONE', #11543, 8.250000000000001776 ) ;
#9759 = CARTESIAN_POINT ( 'NONE',  ( 0.000000000000000000, 0.000000000000000000, 0.000000000000000000 ) ) ;
#9760 = EDGE_CURVE ( 'NONE', #7877, #11930, #382, .T. ) ;
#9761 = ORIENTED_EDGE ( 'NONE', *, *, #12850, .F. ) ;
#9762 = MANIFOLD_SOLID_BREP ( 'Cut-Extrude3', #11491 ) ;
#9763 = EDGE_LOOP ( 'NONE', ( #9473, #7673, #3020, #5480 ) ) ;
#9764 = FACE_OUTER_BOUND ( 'NONE', #10336, .T. ) ;
#9765 = ORIENTED_EDGE ( 'NONE', *, *, #8301, .F. ) ;
#9766 = CARTESIAN_POINT ( 'NONE',  ( -18.05918829504999934, 10.97290950744599947, 118.8499999999999943 ) ) ;
#9767 = CARTESIAN_POINT ( 'NONE',  ( -19.55918829504999934, 27.40458623260099813, 57.35000000000000142 ) ) ;
#9768 = DIRECTION ( 'NONE',  ( -1.000000000000000000, 0.000000000000000000, 0.000000000000000000 ) ) ;
#9770 = EDGE_LOOP ( 'NONE', ( #1766, #8100, #1208, #1059 ) ) ;
#9769 = ADVANCED_FACE ( 'NONE', ( #9830 ), #12188, .T. ) ;
#9771 = CARTESIAN_POINT ( 'NONE',  ( 16.08092853089229024, 4.500000000000000000, -11.23781208254518660 ) ) ;
#9772 = EDGE_CURVE ( 'NONE', #2628, #5367, #12883, .T. ) ;
#9773 = CARTESIAN_POINT ( 'NONE',  ( -18.05918829504999934, 10.97290950744599947, 64.85000000000000853 ) ) ;
#9774 = LINE ( 'NONE', #10894, #8779 ) ;
#9775 = DIRECTION ( 'NONE',  ( 0.000000000000000000, 0.000000000000000000, -1.000000000000000000 ) ) ;
#9776 = AXIS2_PLACEMENT_3D ( 'NONE', #3545, #2513, #6749 ) ;
#9777 = VECTOR ( 'NONE', #1268, 1000.000000000000000 ) ;
#9778 = VECTOR ( 'NONE', #309, 1000.000000000000000 ) ;
#9779 = UNCERTAINTY_MEASURE_WITH_UNIT (LENGTH_MEASURE( 1.000000000000000082E-05 ), #8310, 'distance_accuracy_value', 'NONE');
#9780 = ORIENTED_EDGE ( 'NONE', *, *, #13638, .F. ) ;
#9781 = CARTESIAN_POINT ( 'NONE',  ( -15.18966715138324020, 30.18239061250415034, 54.47301593183773605 ) ) ;
#9782 = AXIS2_PLACEMENT_3D ( 'NONE', #63, #3356, #1175 ) ;
#9783 = VECTOR ( 'NONE', #12996, 1000.000000000000000 ) ;
#9784 = VECTOR ( 'NONE', #2045, 1000.000000000000000 ) ;
#9785 = EDGE_LOOP ( 'NONE', ( #970, #10533, #7574, #7809 ) ) ;
#9786 = CARTESIAN_POINT ( 'NONE',  ( -41.50918829505000218, 27.97290950744599769, 5.250000000000000000 ) ) ;
#9787 = CIRCLE ( 'NONE', #2896, 6.450000000000001066 ) ;
#9788 = PLANE ( 'NONE',  #8939 ) ;
#9789 = CARTESIAN_POINT ( 'NONE',  ( -18.05918829504999934, 7.130333642789880244, 83.57661607529820458 ) ) ;
#9790 = ORIENTED_EDGE ( 'NONE', *, *, #7080, .F. ) ;
#9791 = CARTESIAN_POINT ( 'NONE',  ( -32.05918829504999934, 27.97290950744599769, 0.000000000000000000 ) ) ;
#9792 = ADVANCED_FACE ( 'NONE', ( #11016 ), #11077, .F. ) ;
#9793 = EDGE_CURVE ( 'NONE', #6107, #1219, #10947, .T. ) ;
#9794 = FACE_OUTER_BOUND ( 'NONE', #5506, .T. ) ;
#9795 = FACE_BOUND ( 'NONE', #115, .T. ) ;
#9796 = STYLED_ITEM ( 'NONE', ( #4049 ), #13799 ) ;
#9797 = AXIS2_PLACEMENT_3D ( 'NONE', #13334, #12306, #13206 ) ;
#9798 = VECTOR ( 'NONE', #3905, 1000.000000000000000 ) ;
#9799 = VECTOR ( 'NONE', #5473, 1000.000000000000000 ) ;
#9800 = ADVANCED_FACE ( 'NONE', ( #1431 ), #8630, .T. ) ;
#9801 = B_SPLINE_CURVE_WITH_KNOTS ( 'NONE', 3,
 ( #1313, #9496, #9565, #1101, #13743, #12709, #11669, #7378, #8573, #2111, #8902, #3286, #4269 ),
 .UNSPECIFIED., .F., .F.,
 ( 4, 1, 1, 1, 1, 1, 2, 2, 4 ),
 ( 0.000000000000000000, 0.2500000000000021649, 0.3750000000000038303, 0.4375000000000054401, 0.4687500000000050515, 0.4843750000000056621, 0.4921875000000059397, 0.5000000000000062172, 1.000000000000000000 ),
 .UNSPECIFIED. ) ;
#9802 = VERTEX_POINT ( 'NONE', #8907 ) ;
#9803 = ORIENTED_EDGE ( 'NONE', *, *, #6916, .T. ) ;
#9804 = DIRECTION ( 'NONE',  ( 1.000000000000000000, 0.000000000000000000, 0.000000000000000000 ) ) ;
#9805 = EDGE_LOOP ( 'NONE', ( #13484, #5711, #10397, #976 ) ) ;
#9806 = ORIENTED_EDGE ( 'NONE', *, *, #7389, .F. ) ;
#9807 =( NAMED_UNIT ( * ) PLANE_ANGLE_UNIT ( ) SI_UNIT ( $, .RADIAN. ) );
#9808 = DIRECTION ( 'NONE',  ( 1.000000000000000000, 0.000000000000000000, 0.000000000000000000 ) ) ;
#9809 = DIRECTION ( 'NONE',  ( 0.000000000000000000, 1.000000000000000000, 0.000000000000000000 ) ) ;
#9810 = EDGE_CURVE ( 'NONE', #9989, #6506, #3053, .T. ) ;
#9811 = EDGE_LOOP ( 'NONE', ( #8148, #5403, #9085, #7892 ) ) ;
#9812 = FACE_OUTER_BOUND ( 'NONE', #12458, .T. ) ;
#9813 = AXIS2_PLACEMENT_3D ( 'NONE', #1486, #5734, #446 ) ;
#9814 = CARTESIAN_POINT ( 'NONE',  ( -1.059188295049996231, -6.027090492554000534, 64.35000000000000853 ) ) ;
#9815 = FACE_BOUND ( 'NONE', #557, .T. ) ;
#9816 = FACE_OUTER_BOUND ( 'NONE', #3863, .T. ) ;
#9817 = EDGE_CURVE ( 'NONE', #5387, #6884, #7964, .T. ) ;
#9818 = CARTESIAN_POINT ( 'NONE',  ( -40.05918829505000645, 32.97290950744599769, 10.00000000000000000 ) ) ;
#9819 = ORIENTED_EDGE ( 'NONE', *, *, #13569, .F. ) ;
#9820 = EDGE_CURVE ( 'NONE', #8318, #2826, #9758, .T. ) ;
#9821 = ORIENTED_EDGE ( 'NONE', *, *, #12720, .T. ) ;
#9822 = CIRCLE ( 'NONE', #10703, 0.5000000000000000000 ) ;
#9823 = ORIENTED_EDGE ( 'NONE', *, *, #1683, .T. ) ;
#9824 = ORIENTED_EDGE ( 'NONE', *, *, #10133, .T. ) ;
#9825 = CARTESIAN_POINT ( 'NONE',  ( -29.51816008892539855, -2.179141222803634648, 62.14999999999999858 ) ) ;
#9826 = ORIENTED_EDGE ( 'NONE', *, *, #9760, .F. ) ;
#9827 = FACE_OUTER_BOUND ( 'NONE', #4263, .T. ) ;
#9828 = ORIENTED_EDGE ( 'NONE', *, *, #1777, .F. ) ;
#9829 = DIRECTION ( 'NONE',  ( -1.000000000000000000, 0.000000000000000000, 0.000000000000000000 ) ) ;
#9830 = FACE_OUTER_BOUND ( 'NONE', #8924, .T. ) ;
#9831 = EDGE_CURVE ( 'NONE', #6295, #9665, #5508, .T. ) ;
#9832 = CARTESIAN_POINT ( 'NONE',  ( -19.59368177784231335, 30.30953598072430921, 53.36020361897907804 ) ) ;
#9833 = CARTESIAN_POINT ( 'NONE',  ( -7.499999999999996447, -0.5000000000000019984, -65.00000000000000000 ) ) ;
#9834 = EDGE_LOOP ( 'NONE', ( #1416, #10274, #4354, #3601 ) ) ;
#9835 = CARTESIAN_POINT ( 'NONE',  ( -25.89252162804999813, 10.97290950744599947, 60.04999999999999716 ) ) ;
#9836 = LINE ( 'NONE', #107, #260 ) ;
#9837 = CARTESIAN_POINT ( 'NONE',  ( -13.05918829504999756, 10.97290950744599947, 118.8499999999999943 ) ) ;
#9838 = CIRCLE ( 'NONE', #3805, 6.449999999999997513 ) ;
#9839 = CIRCLE ( 'NONE', #5572, 23.22993838181875148 ) ;
#9840 =( NAMED_UNIT ( * ) PLANE_ANGLE_UNIT ( ) SI_UNIT ( $, .RADIAN. ) );
#9841 = CIRCLE ( 'NONE', #5573, 4.750000000000000888 ) ;
#9842 = ORIENTED_EDGE ( 'NONE', *, *, #428, .T. ) ;
#9843 = VECTOR ( 'NONE', #5569, 1000.000000000000000 ) ;
#9844 = EDGE_CURVE ( 'NONE', #2384, #12622, #614, .T. ) ;
#9845 = EDGE_LOOP ( 'NONE', ( #6685, #5762, #9823, #6989 ) ) ;
#9846 = ORIENTED_EDGE ( 'NONE', *, *, #7645, .T. ) ;
#9847 = ORIENTED_EDGE ( 'NONE', *, *, #11591, .F. ) ;
#9848 = AXIS2_PLACEMENT_3D ( 'NONE', #2368, #12955, #3468 ) ;
#9849 = FACE_OUTER_BOUND ( 'NONE', #9010, .T. ) ;
#9850 = AXIS2_PLACEMENT_3D ( 'NONE', #10609, #1961, #8571 ) ;
#9851 = AXIS2_PLACEMENT_3D ( 'NONE', #5702, #484, #6826 ) ;
#9852 = VERTEX_POINT ( 'NONE', #13441 ) ;
#9853 = LINE ( 'NONE', #10887, #4471 ) ;
#9854 = DIRECTION ( 'NONE',  ( 0.6615960714621565986, -0.7498604124941126159, 0.000000000000000000 ) ) ;
#9855 = CARTESIAN_POINT ( 'NONE',  ( 12.00000000000000000, -2.499999999999999556, -65.00000000000000000 ) ) ;
#9856 = CARTESIAN_POINT ( 'NONE',  ( -24.37001676333060018, -4.028726038184999858, 63.45000000000000284 ) ) ;
#9857 = FACE_BOUND ( 'NONE', #12333, .T. ) ;
#9858 = DIRECTION ( 'NONE',  ( -1.000000000000000000, 0.000000000000000000, 0.000000000000000000 ) ) ;
#9859 = DIRECTION ( 'NONE',  ( -0.7071067811865474617, 8.659560562354903276E-17, 0.7071067811865474617 ) ) ;
#9860 = CARTESIAN_POINT ( 'NONE',  ( 42.63563590245419732, 87.03908161011136713, 0.7500000000000006661 ) ) ;
#9861 = DIRECTION ( 'NONE',  ( 0.000000000000000000, 0.000000000000000000, 1.000000000000000000 ) ) ;
#9862 = AXIS2_PLACEMENT_3D ( 'NONE', #595, #2579, #4792 ) ;
#9863 = ORIENTED_EDGE ( 'NONE', *, *, #12732, .T. ) ;
#9864 = EDGE_CURVE ( 'NONE', #5856, #6747, #8130, .T. ) ;
#9865 = CARTESIAN_POINT ( 'NONE',  ( -17.23229456089049805, 30.34555471844711505, 53.09492650809716707 ) ) ;
#9866 = DIRECTION ( 'NONE',  ( 0.000000000000000000, 0.000000000000000000, 1.000000000000000000 ) ) ;
#9867 = VECTOR ( 'NONE', #4268, 1000.000000000000000 ) ;
#9868 = FACE_OUTER_BOUND ( 'NONE', #11450, .T. ) ;
#9869 = AXIS2_PLACEMENT_3D ( 'NONE', #442, #11004, #12039 ) ;
#9870 = CYLINDRICAL_SURFACE ( 'NONE', #2507, 4.749999999999997335 ) ;
#9871 = AXIS2_PLACEMENT_3D ( 'NONE', #154, #12871, #1007 ) ;
#9872 = FACE_OUTER_BOUND ( 'NONE', #8941, .T. ) ;
#9873 = DIRECTION ( 'NONE',  ( 0.000000000000000000, 0.000000000000000000, 1.000000000000000000 ) ) ;
#9874 = FACE_BOUND ( 'NONE', #7462, .T. ) ;
#9875 = MECHANICAL_DESIGN_GEOMETRIC_PRESENTATION_REPRESENTATION (  '', ( #7617 ), #2535 ) ;
#9876 = ORIENTED_EDGE ( 'NONE', *, *, #11377, .F. ) ;
#9877 = EDGE_CURVE ( 'NONE', #12198, #6660, #2849, .T. ) ;
#9878 = EDGE_LOOP ( 'NONE', ( #685, #4082, #6423, #6811 ) ) ;
#9879 = CARTESIAN_POINT ( 'NONE',  ( -18.05918829504999934, 10.97290950744599947, 57.35000000000000142 ) ) ;
#9880 = VERTEX_POINT ( 'NONE', #9111 ) ;
#9881 = ORIENTED_EDGE ( 'NONE', *, *, #3685, .T. ) ;
#9882 = ORIENTED_EDGE ( 'NONE', *, *, #3243, .F. ) ;
#9883 = VERTEX_POINT ( 'NONE', #13647 ) ;
#9884 = VERTEX_POINT ( 'NONE', #654 ) ;
#9885 = CARTESIAN_POINT ( 'NONE',  ( -18.05918829504999934, 10.97290950744599947, 27.09999999999999787 ) ) ;
#9886 = CARTESIAN_POINT ( 'NONE',  ( -0.04028432657539327000, 4.500000000000000000, 18.54539866546729243 ) ) ;
#9887 = ORIENTED_EDGE ( 'NONE', *, *, #13801, .T. ) ;
#9888 = DIRECTION ( 'NONE',  ( 1.000000000000000000, 0.000000000000000000, 0.000000000000000000 ) ) ;
#9889 = PRESENTATION_LAYER_ASSIGNMENT (  '', '', ( #11889 ) ) ;
#9890 = FACE_OUTER_BOUND ( 'NONE', #4400, .T. ) ;
#9891 = CARTESIAN_POINT ( 'NONE',  ( -1.059188295049996231, -6.027090492554000534, 64.85000000000000853 ) ) ;
#9892 = EDGE_CURVE ( 'NONE', #2367, #11937, #11349, .T. ) ;
#9893 = AXIS2_PLACEMENT_3D ( 'NONE', #12984, #1986, #5431 ) ;
#9894 = FACE_OUTER_BOUND ( 'NONE', #8024, .T. ) ;
#9895 = EDGE_LOOP ( 'NONE', ( #4218, #3880, #10715, #1957 ) ) ;
#9896 = DIRECTION ( 'NONE',  ( 0.000000000000000000, 0.000000000000000000, 1.000000000000000000 ) ) ;
#9897 = VERTEX_POINT ( 'NONE', #1640 ) ;
#9898 = CARTESIAN_POINT ( 'NONE',  ( 140.6356359024541973, 108.9054980190242503, 20.00000000000000000 ) ) ;
#9899 = EDGE_CURVE ( 'NONE', #918, #6678, #8210, .T. ) ;
#9900 = CARTESIAN_POINT ( 'NONE',  ( -21.30549241498041013, 30.13232420323818062, 59.65220830260756202 ) ) ;
#9901 =( BOUNDED_CURVE ( )  B_SPLINE_CURVE ( 3, ( #11384, #11457, #6285, #5165 ),
 .UNSPECIFIED., .F., .F. ) 
 B_SPLINE_CURVE_WITH_KNOTS ( ( 4, 4 ),
 ( 0.000000000000000000, 1.000000000000000000 ),
 .UNSPECIFIED. ) 
 CURVE ( )  GEOMETRIC_REPRESENTATION_ITEM ( )  RATIONAL_B_SPLINE_CURVE ( ( 0.9565783017328499671, 0.3188594339109500075, 0.3188594339109500075, 0.9565783017328499671 ) ) 
 REPRESENTATION_ITEM ( '' )  );
#9902 = ORIENTED_EDGE ( 'NONE', *, *, #11721, .T. ) ;
#9903 = CARTESIAN_POINT ( 'NONE',  ( 100.2760581142613603, 115.9375248198690826, 10.00000000000000000 ) ) ;
#9904 = PLANE ( 'NONE',  #12027 ) ;
#9905 = DIRECTION ( 'NONE',  ( 0.7071067811865505703, 0.000000000000000000, 0.7071067811865444641 ) ) ;
#9906 = AXIS2_PLACEMENT_3D ( 'NONE', #9177, #12450, #5939 ) ;
#9907 = LINE ( 'NONE', #4525, #2705 ) ;
#9908 = EDGE_CURVE ( 'NONE', #10213, #12141, #6094, .T. ) ;
#9909 = ORIENTED_EDGE ( 'NONE', *, *, #2071, .T. ) ;
#9910 = ORIENTED_EDGE ( 'NONE', *, *, #12475, .T. ) ;
#9911 = VERTEX_POINT ( 'NONE', #8064 ) ;
#9912 = CARTESIAN_POINT ( 'NONE',  ( -38.38077571930826082, 22.44393519180575680, 83.57661607529820458 ) ) ;
#9913 = CARTESIAN_POINT ( 'NONE',  ( 92.63563590245421153, 99.03908161011133870, 19.25000000000000000 ) ) ;
#9914 = VECTOR ( 'NONE', #12516, 1000.000000000000000 ) ;
#9915 = CARTESIAN_POINT ( 'NONE',  ( -18.05918829504999934, 10.97290950744599947, 61.85000000000000142 ) ) ;
#9916 = EDGE_CURVE ( 'NONE', #7299, #9802, #4023, .T. ) ;
#9917 = DIRECTION ( 'NONE',  ( 1.000000000000000000, 0.000000000000000000, 0.000000000000000000 ) ) ;
#9918 = DIRECTION ( 'NONE',  ( 0.000000000000000000, 0.000000000000000000, 1.000000000000000000 ) ) ;
#9919 = PLANE ( 'NONE',  #4735 ) ;
#9920 = CARTESIAN_POINT ( 'NONE',  ( -18.05918829504999934, 10.97290950744599947, 57.35000000000000142 ) ) ;
#9921 = CARTESIAN_POINT ( 'NONE',  ( -25.86749127492460332, 30.80589556422609476, 5.250000000000000000 ) ) ;
#9922 = CARTESIAN_POINT ( 'NONE',  ( -16.64497473267689998, 26.91028695795525039, 56.84999999999999432 ) ) ;
#9923 = CARTESIAN_POINT ( 'NONE',  ( -39.80918829504999934, 27.97290950744599769, 7.250000000000000000 ) ) ;
#9924 = ORIENTED_EDGE ( 'NONE', *, *, #5188, .T. ) ;
#9925 = CARTESIAN_POINT ( 'NONE',  ( 134.6356359024541973, 108.9054980190242503, 23.00000000000000000 ) ) ;
#9926 = ORIENTED_EDGE ( 'NONE', *, *, #80, .T. ) ;
#9927 = DIRECTION ( 'NONE',  ( 0.000000000000000000, 0.000000000000000000, -1.000000000000000000 ) ) ;
#9928 = ADVANCED_FACE ( 'NONE', ( #6028 ), #12396, .T. ) ;
#9929 = DIRECTION ( 'NONE',  ( 1.000000000000000000, 0.000000000000000000, 0.000000000000000000 ) ) ;
#9930 = FILL_AREA_STYLE ('',( #2474 ) ) ;
#9931 = CARTESIAN_POINT ( 'NONE',  ( -18.05918829504999934, 10.97290950744599947, 57.35000000000000142 ) ) ;
#9932 = PLANE ( 'NONE',  #12713 ) ;
#9933 = EDGE_CURVE ( 'NONE', #11152, #4755, #3099, .T. ) ;
#9934 = DIRECTION ( 'NONE',  ( 0.000000000000000000, 0.000000000000000000, -1.000000000000000000 ) ) ;
#9935 = ORIENTED_EDGE ( 'NONE', *, *, #11594, .F. ) ;
#9936 = CIRCLE ( 'NONE', #8367, 0.9499999999999995115 ) ;
#9937 = FACE_OUTER_BOUND ( 'NONE', #10849, .T. ) ;
#9938 = VERTEX_POINT ( 'NONE', #725 ) ;
#9939 = ORIENTED_EDGE ( 'NONE', *, *, #11090, .F. ) ;
#9940 = VERTEX_POINT ( 'NONE', #9255 ) ;
#9941 = CARTESIAN_POINT ( 'NONE',  ( -18.05918829504999934, 3.815137874446000055, 61.70038048199999281 ) ) ;
#9942 = CARTESIAN_POINT ( 'NONE',  ( 0.04028432657539351286, 0.000000000000000000, -20.54539866546728533 ) ) ;
#9943 = ORIENTED_EDGE ( 'NONE', *, *, #12666, .T. ) ;
#9944 = CARTESIAN_POINT ( 'NONE',  ( -18.05918829504999934, 19.07290950615085023, 63.35000000000700027 ) ) ;
#9945 = CARTESIAN_POINT ( 'NONE',  ( 6.940811704950009542, -11.02709049255400053, 10.00000000000000000 ) ) ;
#9946 = EDGE_CURVE ( 'NONE', #2296, #9588, #6160, .T. ) ;
#9947 = DIRECTION ( 'NONE',  ( -0.000000000000000000, -0.000000000000000000, -1.000000000000000000 ) ) ;
#9948 = ADVANCED_FACE ( 'NONE', ( #11419, #3947 ), #8195, .F. ) ;
#9949 = AXIS2_PLACEMENT_3D ( 'NONE', #9759, #184, #12971 ) ;
#9950 = CARTESIAN_POINT ( 'NONE',  ( -5.789834139046019956, -5.598733283342819611, 64.85000000000000853 ) ) ;
#9951 = EDGE_CURVE ( 'NONE', #3112, #1146, #12892, .T. ) ;
#9952 = AXIS2_PLACEMENT_3D ( 'NONE', #802, #4106, #12406 ) ;
#9953 = FACE_OUTER_BOUND ( 'NONE', #4188, .T. ) ;
#9954 = EDGE_LOOP ( 'NONE', ( #1557, #6680, #367, #4001 ) ) ;
#9955 = ORIENTED_EDGE ( 'NONE', *, *, #9651, .F. ) ;
#9956 = SURFACE_STYLE_USAGE ( .BOTH. , #3738 ) ;
#9957 = CARTESIAN_POINT ( 'NONE',  ( -20.63590450610939087, 30.21696533308443122, 60.56576002470140452 ) ) ;
#9958 = ORIENTED_EDGE ( 'NONE', *, *, #8003, .T. ) ;
#9959 = CARTESIAN_POINT ( 'NONE',  ( 3.190811704950004657, -6.027090492554000534, 64.35000000000000853 ) ) ;
#9960 = CARTESIAN_POINT ( 'NONE',  ( 103.4499059006094512, 83.97306027416853169, 10.00000000000000000 ) ) ;
#9961 = PLANE ( 'NONE',  #695 ) ;
#9962 = EDGE_CURVE ( 'NONE', #11490, #2763, #5303, .T. ) ;
#9963 = DIRECTION ( 'NONE',  ( -1.000000000000000000, 0.000000000000000000, 0.000000000000000000 ) ) ;
#9964 =( LENGTH_UNIT ( ) NAMED_UNIT ( * ) SI_UNIT ( .MILLI., .METRE. ) );
#9965 = VERTEX_POINT ( 'NONE', #8540 ) ;
#9966 = ORIENTED_EDGE ( 'NONE', *, *, #8335, .T. ) ;
#9967 = VECTOR ( 'NONE', #3236, 1000.000000000000000 ) ;
#9968 = EDGE_CURVE ( 'NONE', #11622, #7715, #871, .T. ) ;
#9969 = EDGE_CURVE ( 'NONE', #6605, #3062, #2206, .T. ) ;
#9970 = VERTEX_POINT ( 'NONE', #1062 ) ;
#9971 = VERTEX_POINT ( 'NONE', #12803 ) ;
#9972 =( BOUNDED_CURVE ( )  B_SPLINE_CURVE ( 3, ( #3066, #7278, #11568, #7350 ),
 .UNSPECIFIED., .F., .F. ) 
 B_SPLINE_CURVE_WITH_KNOTS ( ( 4, 4 ),
 ( 3.141592653589793116, 4.712388980384689674 ),
 .UNSPECIFIED. ) 
 CURVE ( )  GEOMETRIC_REPRESENTATION_ITEM ( )  RATIONAL_B_SPLINE_CURVE ( ( 1.000000000000000000, 0.8047378541243649375, 0.8047378541243649375, 1.000000000000000000 ) ) 
 REPRESENTATION_ITEM ( '' )  );
#9973 = CARTESIAN_POINT ( 'NONE',  ( -16.40519811639460102, 9.098258476210720147, 67.84999999999999432 ) ) ;
#9974 = FACE_OUTER_BOUND ( 'NONE', #13041, .T. ) ;
#9975 = FACE_OUTER_BOUND ( 'NONE', #8948, .T. ) ;
#9976 = DIRECTION ( 'NONE',  ( 3.441911658684139926E-17, 0.000000000000000000, 1.000000000000000000 ) ) ;
#9977 = TOROIDAL_SURFACE ( 'NONE', #12849, 10.00000000000000000, 2.000000000000000000 ) ;
#9978 = DIRECTION ( 'NONE',  ( 0.000000000000000000, 0.000000000000000000, -1.000000000000000000 ) ) ;
#9979 = CARTESIAN_POINT ( 'NONE',  ( -10.78334210919089919, -7.245613863947199640, 64.85000000000000853 ) ) ;
#9980 = CYLINDRICAL_SURFACE ( 'NONE', #1376, 1.999999999999991340 ) ;
#9981 = DIRECTION ( 'NONE',  ( 0.000000000000000000, 0.000000000000000000, 1.000000000000000000 ) ) ;
#9982 = CARTESIAN_POINT ( 'NONE',  ( 4.000000000000001776, 2.000000000000000000, 0.000000000000000000 ) ) ;
#9983 = DIRECTION ( 'NONE',  ( 0.000000000000000000, 1.000000000000000000, 0.000000000000000000 ) ) ;
#9984 = EDGE_CURVE ( 'NONE', #9584, #3775, #5320, .T. ) ;
#9985 = DIRECTION ( 'NONE',  ( 1.000000000000000000, 0.000000000000000000, 0.000000000000000000 ) ) ;
#9986 = DIRECTION ( 'NONE',  ( 1.000000000000000000, 0.000000000000000000, 0.000000000000000000 ) ) ;
#9987 = ADVANCED_FACE ( 'NONE', ( #8678 ), #7752, .T. ) ;
#9988 = EDGE_CURVE ( 'NONE', #7736, #10331, #7083, .T. ) ;
#9989 = VERTEX_POINT ( 'NONE', #3254 ) ;
#9990 = VERTEX_POINT ( 'NONE', #13707 ) ;
#9991 = FACE_BOUND ( 'NONE', #11524, .T. ) ;
#9992 = VERTEX_POINT ( 'NONE', #8605 ) ;
#9993 = ORIENTED_EDGE ( 'NONE', *, *, #6271, .F. ) ;
#9994 = DIRECTION ( 'NONE',  ( -1.000000000000000000, 0.000000000000000000, 0.000000000000000000 ) ) ;
#9995 = PLANE ( 'NONE',  #1803 ) ;
#9996 = CIRCLE ( 'NONE', #3971, 6.449999999999997513 ) ;
#9997 = DIRECTION ( 'NONE',  ( -1.000000000000000000, 0.000000000000000000, 0.000000000000000000 ) ) ;
#9998 = AXIS2_PLACEMENT_3D ( 'NONE', #10574, #4873, #4224 ) ;
#9999 = CARTESIAN_POINT ( 'NONE',  ( -7.241070169793059286, -7.867426463707969830, 17.25000000000000000 ) ) ;
#10000 = AXIS2_PLACEMENT_3D ( 'NONE', #8771, #7700, #4787 ) ;
#10001 = LINE ( 'NONE', #2476, #7793 ) ;
#10002 = CARTESIAN_POINT ( 'NONE',  ( 134.6356359024541973, 108.9054980190242503, 20.00000000000000000 ) ) ;
#10003 = ADVANCED_FACE ( 'NONE', ( #7460 ), #5390, .T. ) ;
#10004 = ORIENTED_EDGE ( 'NONE', *, *, #7266, .F. ) ;
#10005 = AXIS2_PLACEMENT_3D ( 'NONE', #11469, #1906, #6145 ) ;
#10006 = AXIS2_PLACEMENT_3D ( 'NONE', #9920, #6765, #6894 ) ;
#10007 = AXIS2_PLACEMENT_3D ( 'NONE', #9317, #863, #5124 ) ;
#10008 = CARTESIAN_POINT ( 'NONE',  ( -34.25918829536686872, 19.07290950803865215, 63.35000000001154774 ) ) ;
#10009 = ORIENTED_EDGE ( 'NONE', *, *, #11566, .T. ) ;
#10010 = ORIENTED_EDGE ( 'NONE', *, *, #9369, .F. ) ;
#10011 = ORIENTED_EDGE ( 'NONE', *, *, #11452, .F. ) ;
#10012 = VERTEX_POINT ( 'NONE', #7538 ) ;
#10013 = LINE ( 'NONE', #438, #6652 ) ;
#10014 = FACE_OUTER_BOUND ( 'NONE', #11308, .T. ) ;
#10015 = EDGE_LOOP ( 'NONE', ( #11898, #5131, #3865, #11707 ) ) ;
#10016 = DIRECTION ( 'NONE',  ( 1.000000000000000000, 0.000000000000000000, 0.000000000000000000 ) ) ;
#10017 = AXIS2_PLACEMENT_3D ( 'NONE', #8017, #12292, #9986 ) ;
#10018 = CARTESIAN_POINT ( 'NONE',  ( -17.33982109643458003, 26.95666986121975484, 56.03305621834116579 ) ) ;
#10019 = AXIS2_PLACEMENT_3D ( 'NONE', #12522, #708, #2978 ) ;
#10020 = AXIS2_PLACEMENT_3D ( 'NONE', #3013, #4116, #5907 ) ;
#10021 = CYLINDRICAL_SURFACE ( 'NONE', #4020, 4.250000000000000000 ) ;
#10022 = AXIS2_PLACEMENT_3D ( 'NONE', #846, #2979, #7192 ) ;
#10023 = DIRECTION ( 'NONE',  ( 1.000000000000000000, 0.000000000000000000, 0.000000000000000000 ) ) ;
#10024 = VERTEX_POINT ( 'NONE', #11827 ) ;
#10025 = VERTEX_POINT ( 'NONE', #6447 ) ;
#10026 =( GEOMETRIC_REPRESENTATION_CONTEXT ( 3 ) GLOBAL_UNCERTAINTY_ASSIGNED_CONTEXT ( ( #6118 ) ) GLOBAL_UNIT_ASSIGNED_CONTEXT ( ( #9964, #4587, #10958 ) ) REPRESENTATION_CONTEXT ( 'NONE', 'WORKASPACE' ) );
#10027 = EDGE_CURVE ( 'NONE', #1852, #12322, #2214, .T. ) ;
#10028 = ORIENTED_EDGE ( 'NONE', *, *, #6223, .T. ) ;
#10029 = ORIENTED_EDGE ( 'NONE', *, *, #12613, .T. ) ;
#10030 = ADVANCED_FACE ( 'NONE', ( #3388 ), #941, .F. ) ;
#10031 = CIRCLE ( 'NONE', #10690, 1.999999999999986233 ) ;
#10032 = DIRECTION ( 'NONE',  ( 0.000000000000000000, -0.000000000000000000, 1.000000000000000000 ) ) ;
#10033 = VECTOR ( 'NONE', #294, 1000.000000000000000 ) ;
#10034 = ORIENTED_EDGE ( 'NONE', *, *, #8687, .F. ) ;
#10035 = EDGE_CURVE ( 'NONE', #4386, #4017, #5093, .T. ) ;
#10036 = DIRECTION ( 'NONE',  ( 0.000000000000000000, 0.000000000000000000, -1.000000000000000000 ) ) ;
#10037 = CARTESIAN_POINT ( 'NONE',  ( -21.57405949846663873, 30.09282919895730046, 55.62766450024737708 ) ) ;
#10038 = FILL_AREA_STYLE_COLOUR ( '', #7627 ) ;
#10039 = CARTESIAN_POINT ( 'NONE',  ( -35.05918829505000645, 27.97290950744599769, 64.85000000000000853 ) ) ;
#10040 = DIRECTION ( 'NONE',  ( 0.000000000000000000, -1.000000000000000000, 0.000000000000000000 ) ) ;
#10041 = DIRECTION ( 'NONE',  ( 1.000000000000000000, 1.460819769243626736E-15, 0.000000000000000000 ) ) ;
#10042 = CARTESIAN_POINT ( 'NONE',  ( -1.059188295049996231, 27.97290950744599769, 17.25000000000000000 ) ) ;
#10043 = ORIENTED_EDGE ( 'NONE', *, *, #9264, .T. ) ;
#10044 = AXIS2_PLACEMENT_3D ( 'NONE', #1024, #47, #5215 ) ;
#10045 = AXIS2_PLACEMENT_3D ( 'NONE', #11197, #7052, #7122 ) ;
#10046 = EDGE_CURVE ( 'NONE', #8617, #7771, #9731, .T. ) ;
#10047 = ORIENTED_EDGE ( 'NONE', *, *, #6744, .F. ) ;
#10048 = CARTESIAN_POINT ( 'NONE',  ( 0.000000000000000000, 0.000000000000000000, -43.00000000000000000 ) ) ;
#10049 = CARTESIAN_POINT ( 'NONE',  ( 42.63563590245419732, 111.0390816101113387, 19.25000000000000000 ) ) ;
#10050 = ORIENTED_EDGE ( 'NONE', *, *, #9319, .F. ) ;
#10051 = CARTESIAN_POINT ( 'NONE',  ( 44.63563590245421864, 85.03908161011133870, 19.25000000000000000 ) ) ;
#10052 = DIRECTION ( 'NONE',  ( 0.6615960714621574867, -0.7498604124941119498, 0.000000000000000000 ) ) ;
#10053 = DIRECTION ( 'NONE',  ( -0.4528443260392610581, -0.8915896008669277339, 0.000000000000000000 ) ) ;
#10054 = CYLINDRICAL_SURFACE ( 'NONE', #2057, 0.7500000000000072164 ) ;
#10055 = VECTOR ( 'NONE', #11115, 999.9999999999998863 ) ;
#10056 = AXIS2_PLACEMENT_3D ( 'NONE', #13018, #13230, #7906 ) ;
#10057 = CARTESIAN_POINT ( 'NONE',  ( -18.05918829504999934, 7.130333642789880244, 17.25000000000000000 ) ) ;
#10058 = CARTESIAN_POINT ( 'NONE',  ( -1.059188295049996231, -6.027090492554000534, 64.85000000000000853 ) ) ;
#10059 = CARTESIAN_POINT ( 'NONE',  ( -12.81426999815532497, 15.06602133594271820, -3.000000000000000000 ) ) ;
#10060 = PLANE ( 'NONE',  #12061 ) ;
#10061 = PRODUCT_DEFINITION ( 'UNKNOWN', '', #8676, #12566 ) ;
#10062 = FACE_OUTER_BOUND ( 'NONE', #187, .T. ) ;
#10063 = CARTESIAN_POINT ( 'NONE',  ( -5.309188295050000228, -6.027090492554000534, 64.85000000000000853 ) ) ;
#10064 = AXIS2_PLACEMENT_3D ( 'NONE', #1653, #9336, #11432 ) ;
#10065 = CIRCLE ( 'NONE', #9382, 4.749999999999997335 ) ;
#10066 = AXIS2_PLACEMENT_3D ( 'NONE', #13115, #6618, #10893 ) ;
#10067 = EDGE_CURVE ( 'NONE', #129, #11446, #149, .T. ) ;
#10068 = CARTESIAN_POINT ( 'NONE',  ( -27.49999999999998934, 0.000000000000000000, 29.99999999999999645 ) ) ;
#10069 = ORIENTED_EDGE ( 'NONE', *, *, #11732, .F. ) ;
#10070 = DIRECTION ( 'NONE',  ( 1.000000000000000000, 0.000000000000000000, 0.000000000000000000 ) ) ;
#10071 = EDGE_CURVE ( 'NONE', #13343, #2711, #1071, .T. ) ;
#10072 = DIRECTION ( 'NONE',  ( 0.000000000000000000, 0.000000000000000000, 1.000000000000000000 ) ) ;
#10073 = PLANE ( 'NONE',  #929 ) ;
#10074 = ORIENTED_EDGE ( 'NONE', *, *, #12496, .T. ) ;
#10075 = CARTESIAN_POINT ( 'NONE',  ( -4.499999999999999112, -0.5000000000000009992, 0.000000000000000000 ) ) ;
#10076 = EDGE_CURVE ( 'NONE', #2084, #8048, #6237, .T. ) ;
#10077 = AXIS2_PLACEMENT_3D ( 'NONE', #12881, #5469, #3330 ) ;
#10078 = CIRCLE ( 'NONE', #6261, 6.449999999999997513 ) ;
#10079 = CARTESIAN_POINT ( 'NONE',  ( -34.49120980104999035, 19.18892026044596832, 63.36264408499989287 ) ) ;
#10080 = CIRCLE ( 'NONE', #10293, 0.7499999999999966693 ) ;
#10081 = DIRECTION ( 'NONE',  ( -1.000000000000000000, 0.000000000000000000, 0.000000000000000000 ) ) ;
#10082 = CARTESIAN_POINT ( 'NONE',  ( -18.05918829504999934, 10.97290950744599947, 27.09999999999999787 ) ) ;
#10083 = ORIENTED_EDGE ( 'NONE', *, *, #5254, .F. ) ;
#10084 = EDGE_CURVE ( 'NONE', #3512, #11310, #2137, .T. ) ;
#10085 = VECTOR ( 'NONE', #3238, 1000.000000000000000 ) ;
#10086 = CARTESIAN_POINT ( 'NONE',  ( -16.62028905529726330, 30.31569702815750134, 61.38640438266109101 ) ) ;
#10087 = VECTOR ( 'NONE', #745, 1000.000000000000000 ) ;
#10088 = AXIS2_PLACEMENT_3D ( 'NONE', #12343, #11286, #2789 ) ;
#10089 = ORIENTED_EDGE ( 'NONE', *, *, #2971, .F. ) ;
#10090 = ORIENTED_EDGE ( 'NONE', *, *, #11023, .T. ) ;
#10091 = CARTESIAN_POINT ( 'NONE',  ( 0.000000000000000000, 0.000000000000000000, 7.000000000000000000 ) ) ;
#10092 = ORIENTED_EDGE ( 'NONE', *, *, #13036, .F. ) ;
#10093 = CARTESIAN_POINT ( 'NONE',  ( -0.04028432657539327000, 0.000000000000000000, 18.54539866546729243 ) ) ;
#10094 = DIRECTION ( 'NONE',  ( 0.000000000000000000, 2.732534507816520408E-15, 1.000000000000000000 ) ) ;
#10095 = VERTEX_POINT ( 'NONE', #7337 ) ;
#10096 = EDGE_CURVE ( 'NONE', #13375, #12141, #4207, .T. ) ;
#10097 = CARTESIAN_POINT ( 'NONE',  ( 8.000000000000001776, 2.000000000000000000, 0.000000000000000000 ) ) ;
#10098 = CARTESIAN_POINT ( 'NONE',  ( -14.95720466168106100, 17.08029827338444662, 63.64999999999999858 ) ) ;
#10099 = DIRECTION ( 'NONE',  ( 0.000000000000000000, 0.000000000000000000, 1.000000000000000000 ) ) ;
#10100 = CARTESIAN_POINT ( 'NONE',  ( 123.1053058165639555, 68.56941169600116837, 0.7500000000000000000 ) ) ;
#10101 = MECHANICAL_DESIGN_GEOMETRIC_PRESENTATION_REPRESENTATION (  '', ( #5381 ), #37 ) ;
#10102 = ORIENTED_EDGE ( 'NONE', *, *, #1810, .F. ) ;
#10103 = CIRCLE ( 'NONE', #1846, 3.000000000000000000 ) ;
#10104 = CARTESIAN_POINT ( 'NONE',  ( 44.73918929304747394, 108.8019446284309737, 23.00000000000000000 ) ) ;
#10105 = ORIENTED_EDGE ( 'NONE', *, *, #4968, .F. ) ;
#10106 = DIRECTION ( 'NONE',  ( 1.000000000000000000, 0.000000000000000000, 0.000000000000000000 ) ) ;
#10107 = CARTESIAN_POINT ( 'NONE',  ( -21.17876435844129546, 30.15001770343124221, 59.87185067995086740 ) ) ;
#10108 = ORIENTED_EDGE ( 'NONE', *, *, #3550, .T. ) ;
#10109 =( GEOMETRIC_REPRESENTATION_CONTEXT ( 3 ) GLOBAL_UNCERTAINTY_ASSIGNED_CONTEXT ( ( #7943 ) ) GLOBAL_UNIT_ASSIGNED_CONTEXT ( ( #9239, #6988, #10153 ) ) REPRESENTATION_CONTEXT ( 'NONE', 'WORKASPACE' ) );
#10110 = CYLINDRICAL_SURFACE ( 'NONE', #8990, 6.850000000000002309 ) ;
#10111 = DIRECTION ( 'NONE',  ( 0.000000000000000000, 0.000000000000000000, 1.000000000000000000 ) ) ;
#10112 = CARTESIAN_POINT ( 'NONE',  ( -43.05918829505002066, 32.97290950744599769, 10.00000000000000000 ) ) ;
#10113 = DIRECTION ( 'NONE',  ( -0.000000000000000000, 1.000000000000000000, -0.000000000000000000 ) ) ;
#10114 = DIRECTION ( 'NONE',  ( -0.000000000000000000, -0.000000000000000000, 1.000000000000000000 ) ) ;
#10115 = CARTESIAN_POINT ( 'NONE',  ( 0.000000000000000000, 0.000000000000000000, 0.000000000000000000 ) ) ;
#10116 = ORIENTED_EDGE ( 'NONE', *, *, #9309, .F. ) ;
#10117 = EDGE_CURVE ( 'NONE', #129, #11449, #4418, .T. ) ;
#10118 = VECTOR ( 'NONE', #3313, 1000.000000000000000 ) ;
#10119 = DIRECTION ( 'NONE',  ( 0.3132098788326420080, 0.9496839325805410681, 0.000000000000000000 ) ) ;
#10120 = CARTESIAN_POINT ( 'NONE',  ( -39.80918829504999934, -6.027090492554000534, 68.85549045786049760 ) ) ;
#10121 = EDGE_LOOP ( 'NONE', ( #11703, #10287, #7494 ) ) ;
#10122 = DIRECTION ( 'NONE',  ( 1.000000000000000000, -0.000000000000000000, -0.000000000000000000 ) ) ;
#10123 = CARTESIAN_POINT ( 'NONE',  ( 44.63563590245423285, 113.0390816101113387, 19.68933982822018081 ) ) ;
#10124 = DIRECTION ( 'NONE',  ( 0.000000000000000000, 0.000000000000000000, -1.000000000000000000 ) ) ;
#10125 = VECTOR ( 'NONE', #6792, 1000.000000000000000 ) ;
#10126 = FACE_OUTER_BOUND ( 'NONE', #7848, .T. ) ;
#10127 = LINE ( 'NONE', #8790, #10757 ) ;
#10128 = DIRECTION ( 'NONE',  ( -1.000000000000000000, 0.000000000000000000, 0.000000000000000000 ) ) ;
#10129 = DIRECTION ( 'NONE',  ( 1.000000000000000000, -0.000000000000000000, -0.000000000000000000 ) ) ;
#10130 = FACE_OUTER_BOUND ( 'NONE', #5449, .T. ) ;
#10131 = DIRECTION ( 'NONE',  ( 1.000000000000000000, 0.000000000000000000, 0.000000000000000000 ) ) ;
#10132 = DIRECTION ( 'NONE',  ( 1.000000000000000000, 0.000000000000000000, 0.000000000000000000 ) ) ;
#10133 = EDGE_CURVE ( 'NONE', #1440, #1848, #4712, .T. ) ;
#10134 = VECTOR ( 'NONE', #12151, 1000.000000000000000 ) ;
#10135 = EDGE_LOOP ( 'NONE', ( #8096, #1849, #12067, #12035 ) ) ;
#10136 = CARTESIAN_POINT ( 'NONE',  ( -18.05918829504999934, 10.97290950744599947, 17.25000000000000000 ) ) ;
#10137 = ORIENTED_EDGE ( 'NONE', *, *, #13794, .F. ) ;
#10138 = CARTESIAN_POINT ( 'NONE',  ( 68.49370948373500312, 112.2890816101113387, 0.7500000000000006661 ) ) ;
#10139 = DIRECTION ( 'NONE',  ( -0.000000000000000000, -0.000000000000000000, 1.000000000000000000 ) ) ;
#10140 = ORIENTED_EDGE ( 'NONE', *, *, #5166, .T. ) ;
#10141 = DIRECTION ( 'NONE',  ( 0.000000000000000000, 0.000000000000000000, -1.000000000000000000 ) ) ;
#10142 = CARTESIAN_POINT ( 'NONE',  ( -34.21925492805003444, 19.05294282444601706, 63.34900083300006202 ) ) ;
#10143 = DIRECTION ( 'NONE',  ( 0.000000000000000000, 0.000000000000000000, -1.000000000000000000 ) ) ;
#10144 = EDGE_CURVE ( 'NONE', #7594, #11171, #10899, .T. ) ;
#10145 = CARTESIAN_POINT ( 'NONE',  ( -18.05918829504999934, 10.97290950744599947, 24.10000000000000142 ) ) ;
#10146 = EDGE_CURVE ( 'NONE', #4307, #8435, #1525, .T. ) ;
#10147 = EDGE_CURVE ( 'NONE', #5468, #3420, #2440, .T. ) ;
#10148 = VERTEX_POINT ( 'NONE', #9942 ) ;
#10149 = ADVANCED_FACE ( 'NONE', ( #10014 ), #6729, .T. ) ;
#10150 = DIRECTION ( 'NONE',  ( 0.000000000000000000, 0.000000000000000000, 1.000000000000000000 ) ) ;
#10151 = VERTEX_POINT ( 'NONE', #370 ) ;
#10152 = ORIENTED_EDGE ( 'NONE', *, *, #9449, .T. ) ;
#10153 =( NAMED_UNIT ( * ) SI_UNIT ( $, .STERADIAN. ) SOLID_ANGLE_UNIT ( ) );
#10154 = VERTEX_POINT ( 'NONE', #5730 ) ;
#10155 = CARTESIAN_POINT ( 'NONE',  ( -18.05918829504999934, 10.97290950744599947, 14.00000000000000000 ) ) ;
#10156 = DIRECTION ( 'NONE',  ( 0.000000000000000000, 0.000000000000000000, 1.000000000000000000 ) ) ;
#10157 = DIRECTION ( 'NONE',  ( 1.000000000000000000, 0.000000000000000000, 0.000000000000000000 ) ) ;
#10158 = PLANE ( 'NONE',  #8068 ) ;
#10159 = DIRECTION ( 'NONE',  ( -0.000000000000000000, -0.000000000000000000, -1.000000000000000000 ) ) ;
#10160 = CARTESIAN_POINT ( 'NONE',  ( 16.04064420431708982, 4.500000000000000000, 7.307586582922142249 ) ) ;
#10161 = EDGE_CURVE ( 'NONE', #6357, #129, #10670, .T. ) ;
#10162 = DIRECTION ( 'NONE',  ( -1.000000000000000000, 0.000000000000000000, 0.000000000000000000 ) ) ;
#10163 = CIRCLE ( 'NONE', #101, 17.00000000000000355 ) ;
#10164 = EDGE_CURVE ( 'NONE', #2082, #8965, #10439, .T. ) ;
#10165 = ORIENTED_EDGE ( 'NONE', *, *, #1151, .F. ) ;
#10166 = EDGE_CURVE ( 'NONE', #9880, #9471, #413, .T. ) ;
#10167 = ORIENTED_EDGE ( 'NONE', *, *, #4848, .T. ) ;
#10168 = ORIENTED_EDGE ( 'NONE', *, *, #12767, .T. ) ;
#10169 = LINE ( 'NONE', #4850, #12640 ) ;
#10170 = EDGE_LOOP ( 'NONE', ( #11316, #12121, #638, #11480 ) ) ;
#10171 = CARTESIAN_POINT ( 'NONE',  ( -13.53074503465739831, 19.88880551611529768, 62.85000000000000142 ) ) ;
#10172 = TOROIDAL_SURFACE ( 'NONE', #3480, 16.66282263685194920, 1.000000000000000000 ) ;
#10173 = CARTESIAN_POINT ( 'NONE',  ( -20.88744887221551494, 30.18746625240332904, 60.27899883312479545 ) ) ;
#10174 = DIRECTION ( 'NONE',  ( -1.000000000000000000, 0.000000000000000000, 0.000000000000000000 ) ) ;
#10175 = DIRECTION ( 'NONE',  ( -1.000000000000000000, 0.000000000000000000, 0.000000000000000000 ) ) ;
#10176 = DIRECTION ( 'NONE',  ( 0.000000000000000000, 0.000000000000000000, -1.000000000000000000 ) ) ;
#10177 = CARTESIAN_POINT ( 'NONE',  ( 7.500000000000000000, -1.762812401309176307E-15, -65.00000000000000000 ) ) ;
#10178 = DIRECTION ( 'NONE',  ( 1.734723475976807094E-18, -1.000000000000000000, 0.000000000000000000 ) ) ;
#10179 = ORIENTED_EDGE ( 'NONE', *, *, #14, .F. ) ;
#10180 = VECTOR ( 'NONE', #11151, 999.9999999999998863 ) ;
#10181 = EDGE_CURVE ( 'NONE', #9710, #7171, #5664, .T. ) ;
#10182 = ORIENTED_EDGE ( 'NONE', *, *, #10802, .F. ) ;
#10183 = CARTESIAN_POINT ( 'NONE',  ( -10.78334210919089919, -7.245613863947189870, 7.250000000000000000 ) ) ;
#10184 = PLANE ( 'NONE',  #4913 ) ;
#10185 = ORIENTED_EDGE ( 'NONE', *, *, #447, .T. ) ;
#10186 = DIRECTION ( 'NONE',  ( -1.000000000000000000, 0.000000000000000000, 0.000000000000000000 ) ) ;
#10187 = CARTESIAN_POINT ( 'NONE',  ( 44.63563590245422574, 113.0390816101113387, 20.00000000000000000 ) ) ;
#10188 = LINE ( 'NONE', #605, #8199 ) ;
#10189 = CARTESIAN_POINT ( 'NONE',  ( -12.00000000000000000, -2.500000000000000444, -65.00000000000000000 ) ) ;
#10190 = CARTESIAN_POINT ( 'NONE',  ( -10.78334210919089919, 29.19143287883919768, 7.250000000000000000 ) ) ;
#10191 = CARTESIAN_POINT ( 'NONE',  ( 0.000000000000000000, 0.000000000000000000, 0.000000000000000000 ) ) ;
#10192 = CARTESIAN_POINT ( 'NONE',  ( -18.05918829309690210, 18.59099508048574734, 61.65955166400529919 ) ) ;
#10193 = CARTESIAN_POINT ( 'NONE',  ( -1.059188295049996231, -6.027090492554000534, 64.35000000000000853 ) ) ;
#10194 = VECTOR ( 'NONE', #5742, 1000.000000000000000 ) ;
#10195 = CARTESIAN_POINT ( 'NONE',  ( 100.2760581142613603, 115.9375248198690826, 10.00000000000000000 ) ) ;
#10196 = LINE ( 'NONE', #612, #10461 ) ;
#10197 = UNCERTAINTY_MEASURE_WITH_UNIT (LENGTH_MEASURE( 1.000000000000000082E-05 ), #3271, 'distance_accuracy_value', 'NONE');
#10198 = VERTEX_POINT ( 'NONE', #9028 ) ;
#10199 = AXIS2_PLACEMENT_3D ( 'NONE', #9152, #3648, #12159 ) ;
#10200 = CARTESIAN_POINT ( 'NONE',  ( -11.56214829504999919, 4.475869507446000206, 64.85000000000000853 ) ) ;
#10201 = EDGE_CURVE ( 'NONE', #2189, #2730, #4499, .T. ) ;
#10202 = EDGE_CURVE ( 'NONE', #3775, #4364, #13224, .T. ) ;
#10203 = VERTEX_POINT ( 'NONE', #4565 ) ;
#10204 = ORIENTED_EDGE ( 'NONE', *, *, #6551, .F. ) ;
#10205 = DIRECTION ( 'NONE',  ( -0.000000000000000000, -0.000000000000000000, -1.000000000000000000 ) ) ;
#10206 = FACE_OUTER_BOUND ( 'NONE', #7333, .T. ) ;
#10207 = CARTESIAN_POINT ( 'NONE',  ( 0.04028432657539327000, 4.500000000000000000, -16.54539866546730309 ) ) ;
#10208 = CARTESIAN_POINT ( 'NONE',  ( 92.63563590245421153, 99.03908161011133870, 20.00000000000000000 ) ) ;
#10209 = CARTESIAN_POINT ( 'NONE',  ( -30.48673169511680214, 10.97290950744599947, 17.25000000000000000 ) ) ;
#10210 = DIRECTION ( 'NONE',  ( 0.000000000000000000, 0.000000000000000000, 1.000000000000000000 ) ) ;
#10211 = CONICAL_SURFACE ( 'NONE', #4184, 16.75000000000000355, 0.7853981633974461696 ) ;
#10212 = FACE_OUTER_BOUND ( 'NONE', #2208, .T. ) ;
#10213 = VERTEX_POINT ( 'NONE', #12037 ) ;
#10214 = VERTEX_POINT ( 'NONE', #8818 ) ;
#10215 = CARTESIAN_POINT ( 'NONE',  ( -16.07267548837544879, 30.27520963107377838, 61.07113917507989242 ) ) ;
#10216 = AXIS2_PLACEMENT_3D ( 'NONE', #1204, #4231, #10515 ) ;
#10217 = EDGE_LOOP ( 'NONE', ( #1460, #425, #12639, #3849 ) ) ;
#10218 = EDGE_CURVE ( 'NONE', #380, #2149, #9099, .T. ) ;
#10219 = VERTEX_POINT ( 'NONE', #7834 ) ;
#10220 = CIRCLE ( 'NONE', #5294, 18.50000000000000000 ) ;
#10221 = CARTESIAN_POINT ( 'NONE',  ( 2.262399129208274573, -0.4981161769137525952, 17.25000000000000000 ) ) ;
#10222 = LINE ( 'NONE', #639, #6922 ) ;
#10223 = ORIENTED_EDGE ( 'NONE', *, *, #4589, .F. ) ;
#10224 = EDGE_CURVE ( 'NONE', #11751, #3428, #6853, .T. ) ;
#10225 = DIRECTION ( 'NONE',  ( 0.4528443260392610026, 0.8915896008669278450, 0.000000000000000000 ) ) ;
#10226 = CARTESIAN_POINT ( 'NONE',  ( -38.05918829504999934, 10.97290950744600124, 10.00000000000000000 ) ) ;
#10227 = EDGE_CURVE ( 'NONE', #2836, #10499, #13148, .T. ) ;
#10228 = DIRECTION ( 'NONE',  ( 1.000000000000000000, 0.000000000000000000, 0.000000000000000000 ) ) ;
#10229 = DIRECTION ( 'NONE',  ( -1.000000000000000000, 0.000000000000000000, 0.000000000000000000 ) ) ;
#10230 = CARTESIAN_POINT ( 'NONE',  ( -17.30244591831155887, 27.95705352479190964, 58.66032464001973779 ) ) ;
#10231 = FACE_OUTER_BOUND ( 'NONE', #6312, .T. ) ;
#10232 = AXIS2_PLACEMENT_3D ( 'NONE', #12835, #3288, #7502 ) ;
#10233 = VECTOR ( 'NONE', #3600, 1000.000000000000114 ) ;
#10234 = ORIENTED_EDGE ( 'NONE', *, *, #7727, .T. ) ;
#10235 = ORIENTED_EDGE ( 'NONE', *, *, #4395, .T. ) ;
#10236 = ORIENTED_EDGE ( 'NONE', *, *, #9233, .F. ) ;
#10237 = EDGE_CURVE ( 'NONE', #11902, #7831, #5807, .T. ) ;
#10238 =( GEOMETRIC_REPRESENTATION_CONTEXT ( 3 ) GLOBAL_UNCERTAINTY_ASSIGNED_CONTEXT ( ( #1392 ) ) GLOBAL_UNIT_ASSIGNED_CONTEXT ( ( #1947, #8364, #12627 ) ) REPRESENTATION_CONTEXT ( 'NONE', 'WORKASPACE' ) );
#10239 = AXIS2_PLACEMENT_3D ( 'NONE', #4631, #8890, #7833 ) ;
#10240 = AXIS2_PLACEMENT_3D ( 'NONE', #11791, #8512, #2392 ) ;
#10241 = DIRECTION ( 'NONE',  ( 0.000000000000000000, 0.000000000000000000, -1.000000000000000000 ) ) ;
#10242 = AXIS2_PLACEMENT_3D ( 'NONE', #4285, #6431, #8 ) ;
#10243 = CARTESIAN_POINT ( 'NONE',  ( -18.05918829504999934, 30.36027202460864771, 61.70913974837019822 ) ) ;
#10244 = EDGE_LOOP ( 'NONE', ( #5043, #6497, #12405, #437 ) ) ;
#10245 = LINE ( 'NONE', #9322, #6070 ) ;
#10246 = DIRECTION ( 'NONE',  ( 0.000000000000000000, 0.000000000000000000, 1.000000000000000000 ) ) ;
#10247 = CARTESIAN_POINT ( 'NONE',  ( -13.53074503465739831, 19.88880551611529768, 64.85000000000000853 ) ) ;
#10248 = EDGE_CURVE ( 'NONE', #6548, #8825, #3554, .T. ) ;
#10249 = CARTESIAN_POINT ( 'NONE',  ( -5.809188295050001116, 27.97290950744599769, 68.85549045786049760 ) ) ;
#10250 = ORIENTED_EDGE ( 'NONE', *, *, #8798, .T. ) ;
#10251 = AXIS2_PLACEMENT_3D ( 'NONE', #2928, #8074, #1927 ) ;
#10252 = AXIS2_PLACEMENT_3D ( 'NONE', #1675, #2757, #624 ) ;
#10253 = VECTOR ( 'NONE', #11145, 1000.000000000000000 ) ;
#10254 = EDGE_CURVE ( 'NONE', #6577, #9588, #13783, .T. ) ;
#10255 = DIRECTION ( 'NONE',  ( 0.000000000000000000, 0.000000000000000000, 1.000000000000000000 ) ) ;
#10256 = EDGE_LOOP ( 'NONE', ( #3791, #11223, #3378, #968, #9335 ) ) ;
#10257 = ORIENTED_EDGE ( 'NONE', *, *, #10266, .T. ) ;
#10258 = DIRECTION ( 'NONE',  ( 1.000000000000000000, 0.000000000000000000, 0.000000000000000000 ) ) ;
#10259 = CARTESIAN_POINT ( 'NONE',  ( 43.38563590245419732, 99.03908161011133870, 0.000000000000000000 ) ) ;
#10260 = CARTESIAN_POINT ( 'NONE',  ( -35.05918829505000645, -6.027090492554000534, 7.250000000000000000 ) ) ;
#10261 = DIRECTION ( 'NONE',  ( 1.000000000000000000, -0.000000000000000000, -0.000000000000000000 ) ) ;
#10262 = DIRECTION ( 'NONE',  ( -0.9496839325805410681, 0.3132098788326420080, 0.000000000000000000 ) ) ;
#10263 = CARTESIAN_POINT ( 'NONE',  ( 134.6356359024541973, 94.90549801902425031, 23.00000000000000000 ) ) ;
#10264 = CARTESIAN_POINT ( 'NONE',  ( -39.80918829504999934, -6.027090492554000534, 7.250000000000000000 ) ) ;
#10265 = LINE ( 'NONE', #7871, #6493 ) ;
#10266 = EDGE_CURVE ( 'NONE', #13640, #2183, #12820, .T. ) ;
#10267 = CARTESIAN_POINT ( 'NONE',  ( 0.04028432657539327000, 0.000000000000000000, -18.54539866546729243 ) ) ;
#10268 = VECTOR ( 'NONE', #9179, 1000.000000000000000 ) ;
#10269 = AXIS2_PLACEMENT_3D ( 'NONE', #10177, #2854, #7212 ) ;
#10270 = VERTEX_POINT ( 'NONE', #5111 ) ;
#10271 = AXIS2_PLACEMENT_3D ( 'NONE', #13136, #3585, #7817 ) ;
#10272 = LINE ( 'NONE', #1955, #8378 ) ;
#10273 = EDGE_LOOP ( 'NONE', ( #12016, #271, #13178, #4752, #4826 ) ) ;
#10274 = ORIENTED_EDGE ( 'NONE', *, *, #10084, .F. ) ;
#10275 = DIRECTION ( 'NONE',  ( 0.000000000000000000, 0.000000000000000000, -1.000000000000000000 ) ) ;
#10276 = DIRECTION ( 'NONE',  ( 0.000000000000000000, -0.000000000000000000, 1.000000000000000000 ) ) ;
#10277 = FACE_OUTER_BOUND ( 'NONE', #5708, .T. ) ;
#10278 = CARTESIAN_POINT ( 'NONE',  ( 116.7775623211734342, 112.2890816101113387, 19.25000000000000000 ) ) ;
#10279 = DIRECTION ( 'NONE',  ( 0.000000000000000000, 0.000000000000000000, 1.000000000000000000 ) ) ;
#10280 = CARTESIAN_POINT ( 'NONE',  ( -10.82033510625394079, -2.574630058508199593, 62.14999999999999858 ) ) ;
#10281 = DIRECTION ( 'NONE',  ( -1.000000000000000000, 0.000000000000000000, 0.000000000000000000 ) ) ;
#10282 = CIRCLE ( 'NONE', #10064, 34.69999999999999574 ) ;
#10283 = AXIS2_PLACEMENT_3D ( 'NONE', #6075, #10350, #842 ) ;
#10284 = TOROIDAL_SURFACE ( 'NONE', #6927, 3.000000000000000888, 2.000000000000000000 ) ;
#10285 = ADVANCED_FACE ( 'NONE', ( #4006 ), #2701, .F. ) ;
#10286 = EDGE_LOOP ( 'NONE', ( #13672, #8372, #8246, #12863 ) ) ;
#10287 = ORIENTED_EDGE ( 'NONE', *, *, #4324, .F. ) ;
#10288 = CARTESIAN_POINT ( 'NONE',  ( -15.27956492296077329, 30.19337278779117284, 60.33853848387425245 ) ) ;
#10289 = ORIENTED_EDGE ( 'NONE', *, *, #447, .F. ) ;
#10290 = AXIS2_PLACEMENT_3D ( 'NONE', #72, #3367, #13753 ) ;
#10291 = CARTESIAN_POINT ( 'NONE',  ( 83.82136590429891498, 114.1051029460540605, 20.00000000000000000 ) ) ;
#10292 = EDGE_LOOP ( 'NONE', ( #3516, #1259, #391, #1476 ) ) ;
#10293 = AXIS2_PLACEMENT_3D ( 'NONE', #4177, #10387, #2945 ) ;
#10294 = ORIENTED_EDGE ( 'NONE', *, *, #5935, .T. ) ;
#10295 = DIRECTION ( 'NONE',  ( -1.000000000000000000, 0.000000000000000000, 0.000000000000000000 ) ) ;
#10296 = LINE ( 'NONE', #12448, #12905 ) ;
#10297 = CARTESIAN_POINT ( 'NONE',  ( 134.6356359024541973, 108.9054980190242503, 22.75000000000000000 ) ) ;
#10298 = CARTESIAN_POINT ( 'NONE',  ( -18.05918829504999934, 10.97290950744599947, 64.85000000000000853 ) ) ;
#10299 = CARTESIAN_POINT ( 'NONE',  ( -6.000000000000000888, 7.347880794884120722E-16, -43.00000000000000000 ) ) ;
#10300 = DIRECTION ( 'NONE',  ( 0.000000000000000000, -0.000000000000000000, -1.000000000000000000 ) ) ;
#10301 = ADVANCED_FACE ( 'NONE', ( #5878 ), #8122, .F. ) ;
#10302 = CIRCLE ( 'NONE', #4726, 1.999999999999996669 ) ;
#10303 = VERTEX_POINT ( 'NONE', #13350 ) ;
#10304 = ORIENTED_EDGE ( 'NONE', *, *, #12908, .T. ) ;
#10305 = DIRECTION ( 'NONE',  ( 0.000000000000000000, 0.000000000000000000, 1.000000000000000000 ) ) ;
#10306 = DIRECTION ( 'NONE',  ( 1.000000000000000000, 0.000000000000000000, -0.000000000000000000 ) ) ;
#10307 = CIRCLE ( 'NONE', #11422, 24.92993838181874722 ) ;
#10308 = DIRECTION ( 'NONE',  ( -1.000000000000000000, 0.000000000000000000, 0.000000000000000000 ) ) ;
#10309 = CARTESIAN_POINT ( 'NONE',  ( 116.7775623211734342, 75.03908161011133870, 20.00000000000000000 ) ) ;
#10310 = CARTESIAN_POINT ( 'NONE',  ( 4.599650328638321461, 0.000000000000000000, 5.878124499050807472 ) ) ;
#10311 = FACE_BOUND ( 'NONE', #7733, .T. ) ;
#10312 = SHAPE_DEFINITION_REPRESENTATION ( #2321, #5156 ) ;
#10313 = ORIENTED_EDGE ( 'NONE', *, *, #7820, .F. ) ;
#10314 = EDGE_LOOP ( 'NONE', ( #3216, #7172, #1719, #7679 ) ) ;
#10315 = EDGE_CURVE ( 'NONE', #5819, #510, #10296, .T. ) ;
#10316 = CIRCLE ( 'NONE', #12550, 2.000000000000001776 ) ;
#10317 = EDGE_CURVE ( 'NONE', #12584, #2746, #11351, .T. ) ;
#10318 = DIRECTION ( 'NONE',  ( 0.000000000000000000, 0.000000000000000000, 1.000000000000000000 ) ) ;
#10319 = EDGE_LOOP ( 'NONE', ( #392, #10443, #13675, #11269 ) ) ;
#10320 = ORIENTED_EDGE ( 'NONE', *, *, #2752, .F. ) ;
#10321 = CARTESIAN_POINT ( 'NONE',  ( -18.05918829504999934, 10.97290950744599947, 60.65000000000000568 ) ) ;
#10322 = DIRECTION ( 'NONE',  ( 0.000000000000000000, 0.000000000000000000, -1.000000000000000000 ) ) ;
#10323 = LINE ( 'NONE', #5209, #3829 ) ;
#10324 = FACE_OUTER_BOUND ( 'NONE', #8291, .T. ) ;
#10325 = CARTESIAN_POINT ( 'NONE',  ( -35.05918829504999934, 10.97290950744600124, 12.50000000000000000 ) ) ;
#10326 = CARTESIAN_POINT ( 'NONE',  ( -4.499999999999999112, -1.301042606982605321E-15, 0.000000000000000000 ) ) ;
#10327 = DIRECTION ( 'NONE',  ( 0.000000000000000000, 0.000000000000000000, -1.000000000000000000 ) ) ;
#10328 = AXIS2_PLACEMENT_3D ( 'NONE', #8069, #13576, #7007 ) ;
#10329 = CARTESIAN_POINT ( 'NONE',  ( 50.53208251186094202, 94.80194462843097369, 23.00000000000000000 ) ) ;
#10330 = EDGE_CURVE ( 'NONE', #1108, #2279, #8228, .T. ) ;
#10331 = VERTEX_POINT ( 'NONE', #10226 ) ;
#10332 = EDGE_CURVE ( 'NONE', #12635, #6090, #3111, .T. ) ;
#10333 = ORIENTED_EDGE ( 'NONE', *, *, #4643, .F. ) ;
#10334 = ORIENTED_EDGE ( 'NONE', *, *, #10936, .T. ) ;
#10335 = CARTESIAN_POINT ( 'NONE',  ( -10.25088531517539714, 30.80589556422609832, 5.250000000000000000 ) ) ;
#10336 = EDGE_LOOP ( 'NONE', ( #3147, #12798, #2857, #4181, #11695 ) ) ;
#10337 = VERTEX_POINT ( 'NONE', #11406 ) ;
#10338 = CARTESIAN_POINT ( 'NONE',  ( -19.70293766808219615, 16.19054976041004679, 68.39999137210355684 ) ) ;
#10339 = CARTESIAN_POINT ( 'NONE',  ( 45.16596598834414777, 112.5087515242214238, 0.000000000000000000 ) ) ;
#10340 = DIRECTION ( 'NONE',  ( -0.000000000000000000, -0.000000000000000000, -1.000000000000000000 ) ) ;
#10341 =( BOUNDED_CURVE ( )  B_SPLINE_CURVE ( 3, ( #10404, #12644, #980, #7111 ),
 .UNSPECIFIED., .F., .F. ) 
 B_SPLINE_CURVE_WITH_KNOTS ( ( 4, 4 ),
 ( 0.000000000000000000, 1.570796326794896558 ),
 .UNSPECIFIED. ) 
 CURVE ( )  GEOMETRIC_REPRESENTATION_ITEM ( )  RATIONAL_B_SPLINE_CURVE ( ( 1.000000000000000000, 0.8047378541243649375, 0.8047378541243649375, 1.000000000000000000 ) ) 
 REPRESENTATION_ITEM ( '' )  );
#10342 = DIRECTION ( 'NONE',  ( 1.000000000000000000, 0.000000000000000000, 0.000000000000000000 ) ) ;
#10343 = CYLINDRICAL_SURFACE ( 'NONE', #8929, 0.2500000000000002220 ) ;
#10344 = AXIS2_PLACEMENT_3D ( 'NONE', #4948, #11372, #4119 ) ;
#10345 = ORIENTED_EDGE ( 'NONE', *, *, #11008, .F. ) ;
#10346 = EDGE_CURVE ( 'NONE', #6180, #3595, #13557, .T. ) ;
#10347 = ORIENTED_EDGE ( 'NONE', *, *, #4853, .T. ) ;
#10348 = CARTESIAN_POINT ( 'NONE',  ( -14.87621594265382363, 30.14123926869076442, 54.93378218723427153 ) ) ;
#10349 = ORIENTED_EDGE ( 'NONE', *, *, #206, .T. ) ;
#10350 = DIRECTION ( 'NONE',  ( 0.000000000000000000, 0.000000000000000000, -1.000000000000000000 ) ) ;
#10351 = CARTESIAN_POINT ( 'NONE',  ( -12.00000000000000000, 2.500000000000000000, -65.00000000000000000 ) ) ;
#10352 = ORIENTED_EDGE ( 'NONE', *, *, #1375, .F. ) ;
#10353 = FACE_OUTER_BOUND ( 'NONE', #9024, .T. ) ;
#10354 = CARTESIAN_POINT ( 'NONE',  ( 142.6356359024541973, 87.03908161011133870, 0.7500000000000006661 ) ) ;
#10355 = CYLINDRICAL_SURFACE ( 'NONE', #2272, 3.449999999999999734 ) ;
#10356 = CYLINDRICAL_SURFACE ( 'NONE', #6327, 16.00000000000000355 ) ;
#10357 = DIRECTION ( 'NONE',  ( 1.000000000000000000, 0.000000000000000000, 0.000000000000000000 ) ) ;
#10358 = DIRECTION ( 'NONE',  ( 0.000000000000000000, 0.000000000000000000, 1.000000000000000000 ) ) ;
#10359 = ORIENTED_EDGE ( 'NONE', *, *, #12832, .F. ) ;
#10360 = VERTEX_POINT ( 'NONE', #576 ) ;
#10361 = ORIENTED_EDGE ( 'NONE', *, *, #4934, .T. ) ;
#10362 = ORIENTED_EDGE ( 'NONE', *, *, #8744, .T. ) ;
#10363 = EDGE_CURVE ( 'NONE', #7637, #8318, #2905, .T. ) ;
#10364 = ADVANCED_FACE ( 'NONE', ( #12523 ), #6079, .T. ) ;
#10365 = DIRECTION ( 'NONE',  ( 0.000000000000000000, 0.000000000000000000, 1.000000000000000000 ) ) ;
#10366 = EDGE_LOOP ( 'NONE', ( #6937, #11123, #20, #1901 ) ) ;
#10367 = CARTESIAN_POINT ( 'NONE',  ( -19.61493467298536331, 30.30811942209248500, 61.32902609463271659 ) ) ;
#10368 = CARTESIAN_POINT ( 'NONE',  ( -18.05918829504999934, 10.97290950744599947, 61.85000000000000142 ) ) ;
#10369 = EDGE_CURVE ( 'NONE', #9632, #9965, #641, .T. ) ;
#10370 = DIRECTION ( 'NONE',  ( 1.000000000000000000, 0.000000000000000000, 0.000000000000000000 ) ) ;
#10371 = CYLINDRICAL_SURFACE ( 'NONE', #2745, 17.00000000000000000 ) ;
#10372 = CIRCLE ( 'NONE', #5671, 1.999999999999991340 ) ;
#10373 = CARTESIAN_POINT ( 'NONE',  ( -20.04397650943645459, 13.22249074492834175, 27.09999999999999787 ) ) ;
#10374 = ORIENTED_EDGE ( 'NONE', *, *, #13482, .F. ) ;
#10375 = EDGE_LOOP ( 'NONE', ( #7017, #1265, #8414, #1896 ) ) ;
#10376 = CIRCLE ( 'NONE', #113, 12.00000000000000355 ) ;
#10377 = CARTESIAN_POINT ( 'NONE',  ( -18.05918829504999934, 10.97290950744599947, 60.65000000000000568 ) ) ;
#10378 = ORIENTED_EDGE ( 'NONE', *, *, #4279, .T. ) ;
#10379 = VERTEX_POINT ( 'NONE', #10418 ) ;
#10380 = DIRECTION ( 'NONE',  ( 0.000000000000000000, 0.000000000000000000, 1.000000000000000000 ) ) ;
#10381 = ADVANCED_FACE ( 'NONE', ( #1692 ), #11203, .T. ) ;
#10382 = CARTESIAN_POINT ( 'NONE',  ( 1.653273178848926867E-15, 8.500000000000000000, 13.50000000000000000 ) ) ;
#10383 = CARTESIAN_POINT ( 'NONE',  ( -27.49999999999998934, 9.000000000000000000, -30.00000000000000355 ) ) ;
#10384 = CARTESIAN_POINT ( 'NONE',  ( -22.69945727585292872, 13.54674356991320394, 68.54372738201359994 ) ) ;
#10385 = CYLINDRICAL_SURFACE ( 'NONE', #13357, 23.49999999999999645 ) ;
#10386 = PLANE ( 'NONE',  #9349 ) ;
#10387 = DIRECTION ( 'NONE',  ( -0.7050191076322684935, -0.7091883091770476710, 0.000000000000000000 ) ) ;
#10388 = ADVANCED_FACE ( 'NONE', ( #11470, #3871 ), #5036, .F. ) ;
#10389 = DIRECTION ( 'NONE',  ( 0.000000000000000000, 0.000000000000000000, -1.000000000000000000 ) ) ;
#10390 = FILL_AREA_STYLE ('',( #814 ) ) ;
#10391 = ORIENTED_EDGE ( 'NONE', *, *, #8063, .T. ) ;
#10392 = CIRCLE ( 'NONE', #1239, 0.7499999999999966693 ) ;
#10393 = ORIENTED_EDGE ( 'NONE', *, *, #8156, .F. ) ;
#10394 = ORIENTED_EDGE ( 'NONE', *, *, #11857, .F. ) ;
#10395 = LINE ( 'NONE', #12493, #1684 ) ;
#10396 = ORIENTED_EDGE ( 'NONE', *, *, #6939, .F. ) ;
#10397 = ORIENTED_EDGE ( 'NONE', *, *, #1830, .T. ) ;
#10399 = ADVANCED_FACE ( 'NONE', ( #4911 ), #1907, .F. ) ;
#10398 = VERTEX_POINT ( 'NONE', #9091 ) ;
#10400 = CARTESIAN_POINT ( 'NONE',  ( 0.000000000000000000, 8.500000000000000000, 0.000000000000000000 ) ) ;
#10401 = DIRECTION ( 'NONE',  ( 0.000000000000000000, -1.000000000000000000, 0.000000000000000000 ) ) ;
#10402 = DIRECTION ( 'NONE',  ( -0.000000000000000000, -0.000000000000000000, 1.000000000000000000 ) ) ;
#10403 = CARTESIAN_POINT ( 'NONE',  ( -11.06274345774342116, 24.74796884084004844, 58.54999999999999716 ) ) ;
#10404 = CARTESIAN_POINT ( 'NONE',  ( 134.6356359024541973, 94.90549801902425031, 22.75000000000000000 ) ) ;
#10405 = DIRECTION ( 'NONE',  ( -1.000000000000000000, 0.000000000000000000, 0.000000000000000000 ) ) ;
#10406 = ADVANCED_FACE ( 'NONE', ( #11681 ), #11535, .T. ) ;
#10407 = AXIS2_PLACEMENT_3D ( 'NONE', #11313, #12638, #4959 ) ;
#10408 = ORIENTED_EDGE ( 'NONE', *, *, #12167, .F. ) ;
#10409 = CARTESIAN_POINT ( 'NONE',  ( -14.97129325674108991, 30.15419697592694348, 59.91884240419840069 ) ) ;
#10410 = ORIENTED_EDGE ( 'NONE', *, *, #6699, .F. ) ;
#10411 = EDGE_CURVE ( 'NONE', #12867, #973, #7526, .T. ) ;
#10412 = DIRECTION ( 'NONE',  ( 1.000000000000000000, -0.000000000000000000, 0.000000000000000000 ) ) ;
#10413 = SHAPE_REPRESENTATION ( 'Flange', ( #6434 ), #10026 ) ;
#10414 = FILL_AREA_STYLE ('',( #12652 ) ) ;
#10415 = CYLINDRICAL_SURFACE ( 'NONE', #9405, 6.299999999999999822 ) ;
#10416 = EDGE_LOOP ( 'NONE', ( #6573, #2059, #2531, #13126 ) ) ;
#10417 = CARTESIAN_POINT ( 'NONE',  ( -18.05918829504999934, 14.81548537210212046, 17.25000000000000000 ) ) ;
#10418 = CARTESIAN_POINT ( 'NONE',  ( -7.999999999999996447, -1.701580061351808733E-15, -65.00000000000000000 ) ) ;
#10419 = CIRCLE ( 'NONE', #1048, 6.000000000000000888 ) ;
#10420 = CYLINDRICAL_SURFACE ( 'NONE', #7577, 0.7499999999999973355 ) ;
#10421 = DIRECTION ( 'NONE',  ( 1.000000000000000000, -0.000000000000000000, 0.000000000000000000 ) ) ;
#10422 = DIRECTION ( 'NONE',  ( 0.000000000000000000, 0.000000000000000000, 1.000000000000000000 ) ) ;
#10423 = ADVANCED_FACE ( 'NONE', ( #9510 ), #1047, .F. ) ;
#10424 = CARTESIAN_POINT ( 'NONE',  ( -25.86749127492459976, 30.80589556422609832, 17.25000000000000000 ) ) ;
#10425 = VERTEX_POINT ( 'NONE', #11739 ) ;
#10426 = VERTEX_POINT ( 'NONE', #7326 ) ;
#10427 = AXIS2_PLACEMENT_3D ( 'NONE', #6176, #7478, #7354 ) ;
#10428 = VERTEX_POINT ( 'NONE', #9451 ) ;
#10429 = EDGE_LOOP ( 'NONE', ( #4774, #2624, #1489 ) ) ;
#10430 = ORIENTED_EDGE ( 'NONE', *, *, #8634, .F. ) ;
#10431 = ORIENTED_EDGE ( 'NONE', *, *, #13085, .T. ) ;
#10432 = CARTESIAN_POINT ( 'NONE',  ( 92.63563590245421153, 99.03908161011133870, 0.000000000000000000 ) ) ;
#10433 = CARTESIAN_POINT ( 'NONE',  ( -19.73609606983273324, 30.29966228794214089, 61.26430342259844508 ) ) ;
#10434 = AXIS2_PLACEMENT_3D ( 'NONE', #8758, #3781, #7042 ) ;
#10435 = CARTESIAN_POINT ( 'NONE',  ( -19.55918829504999934, 21.47290950744600124, 57.35000000000000142 ) ) ;
#10436 = AXIS2_PLACEMENT_3D ( 'NONE', #12036, #7613, #1132 ) ;
#10437 = CARTESIAN_POINT ( 'NONE',  ( -16.55918829504999579, 21.47290950744600124, 57.35000000000000142 ) ) ;
#10438 = DIRECTION ( 'NONE',  ( 0.000000000000000000, 0.000000000000000000, 1.000000000000000000 ) ) ;
#10439 = CIRCLE ( 'NONE', #9332, 0.9499999999999995115 ) ;
#10440 = DIRECTION ( 'NONE',  ( 0.000000000000000000, 0.000000000000000000, 1.000000000000000000 ) ) ;
#10441 = DIRECTION ( 'NONE',  ( -6.744604874597825983E-15, 1.000000000000000000, 0.000000000000000000 ) ) ;
#10442 = EDGE_LOOP ( 'NONE', ( #1129, #4371, #12350, #11327 ) ) ;
#10443 = ORIENTED_EDGE ( 'NONE', *, *, #7067, .T. ) ;
#10444 = EDGE_CURVE ( 'NONE', #12702, #12568, #1188, .T. ) ;
#10445 = AXIS2_PLACEMENT_3D ( 'NONE', #5493, #5362, #6557 ) ;
#10446 = CIRCLE ( 'NONE', #2893, 9.999999999999994671 ) ;
#10447 = CIRCLE ( 'NONE', #12234, 2.700000000000001066 ) ;
#10448 = CIRCLE ( 'NONE', #4432, 4.750000000000000000 ) ;
#10449 = DIRECTION ( 'NONE',  ( 0.000000000000000000, 0.000000000000000000, -1.000000000000000000 ) ) ;
#10450 = DIRECTION ( 'NONE',  ( 0.3132098788326367900, -0.9496839325805428444, 0.000000000000000000 ) ) ;
#10451 = VERTEX_POINT ( 'NONE', #1984 ) ;
#10452 = CARTESIAN_POINT ( 'NONE',  ( 103.4499059006094512, 83.97306027416853169, 10.00000000000000000 ) ) ;
#10453 = DIRECTION ( 'NONE',  ( 0.000000000000000000, 0.000000000000000000, 1.000000000000000000 ) ) ;
#10454 = CARTESIAN_POINT ( 'NONE',  ( -32.05918829504999934, -6.027090492554000534, 0.000000000000000000 ) ) ;
#10455 = DIRECTION ( 'NONE',  ( 0.000000000000000000, 0.000000000000000000, 1.000000000000000000 ) ) ;
#10456 = CARTESIAN_POINT ( 'NONE',  ( 16.45469220996245241, 1.832421873814834345, -3.000000000000000000 ) ) ;
#10457 = DIRECTION ( 'NONE',  ( 0.000000000000000000, 0.000000000000000000, -1.000000000000000000 ) ) ;
#10458 = CARTESIAN_POINT ( 'NONE',  ( -40.33164489498318517, 10.97290950744599947, 5.250000000000000000 ) ) ;
#10459 = EDGE_CURVE ( 'NONE', #5367, #2628, #7099, .T. ) ;
#10460 = DIRECTION ( 'NONE',  ( 1.000000000000000000, 0.000000000000000000, 0.000000000000000000 ) ) ;
#10461 = VECTOR ( 'NONE', #4683, 1000.000000000000000 ) ;
#10462 = AXIS2_PLACEMENT_3D ( 'NONE', #9577, #3240, #11952 ) ;
#10463 = VECTOR ( 'NONE', #7254, 1000.000000000000000 ) ;
#10464 = EDGE_CURVE ( 'NONE', #9989, #1735, #10907, .T. ) ;
#10465 = ORIENTED_EDGE ( 'NONE', *, *, #11390, .F. ) ;
#10466 =( REPRESENTATION_RELATIONSHIP ('NONE','NONE', #11848, #13195 ) REPRESENTATION_RELATIONSHIP_WITH_TRANSFORMATION ( #4161 )SHAPE_REPRESENTATION_RELATIONSHIP( ) );
#10467 = ORIENTED_EDGE ( 'NONE', *, *, #4518, .T. ) ;
#10468 = DIRECTION ( 'NONE',  ( 0.000000000000000000, 0.000000000000000000, 1.000000000000000000 ) ) ;
#10469 = VERTEX_POINT ( 'NONE', #9578 ) ;
#10470 = PRODUCT_DEFINITION_FORMATION_WITH_SPECIFIED_SOURCE ( 'ANY', '', #463, .NOT_KNOWN. ) ;
#10471 = ORIENTED_EDGE ( 'NONE', *, *, #9722, .T. ) ;
#10472 = EDGE_LOOP ( 'NONE', ( #11088, #5983, #3704, #10961 ) ) ;
#10473 = CARTESIAN_POINT ( 'NONE',  ( -1.059188295049996231, 27.97290950744599769, 64.85000000000000853 ) ) ;
#10474 = CARTESIAN_POINT ( 'NONE',  ( 134.8856359024541973, 94.65549801902425031, 23.00000000000000000 ) ) ;
#10475 = ADVANCED_FACE ( 'NONE', ( #2191 ), #11607, .T. ) ;
#10476 = DIRECTION ( 'NONE',  ( -0.000000000000000000, 1.000000000000000000, -0.000000000000000000 ) ) ;
#10477 = AXIS2_PLACEMENT_3D ( 'NONE', #5335, #11766, #6462 ) ;
#10478 = CARTESIAN_POINT ( 'NONE',  ( -18.05918829504999934, 10.97290950744599947, 64.85000000000000853 ) ) ;
#10479 = EDGE_CURVE ( 'NONE', #2105, #5663, #12791, .T. ) ;
#10480 = AXIS2_PLACEMENT_3D ( 'NONE', #11386, #8243, #13415 ) ;
#10481 = ORIENTED_EDGE ( 'NONE', *, *, #10598, .T. ) ;
#10482 = CARTESIAN_POINT ( 'NONE',  ( -14.82082868479300508, 30.13344396834445860, 59.66657486885861772 ) ) ;
#10483 = VERTEX_POINT ( 'NONE', #3040 ) ;
#10484 = ORIENTED_EDGE ( 'NONE', *, *, #10459, .T. ) ;
#10485 = CARTESIAN_POINT ( 'NONE',  ( -18.05918829504999934, 10.97290950744599947, 57.35000000000000142 ) ) ;
#10486 = EDGE_CURVE ( 'NONE', #11310, #9517, #3241, .T. ) ;
#10487 = CARTESIAN_POINT ( 'NONE',  ( 140.6356359024541973, 89.90549801902423610, 22.89644660940672694 ) ) ;
#10488 = FACE_OUTER_BOUND ( 'NONE', #1409, .T. ) ;
#10489 = VERTEX_POINT ( 'NONE', #10698 ) ;
#10490 = DIRECTION ( 'NONE',  ( 0.4528443260392608360, 0.8915896008669277339, 0.000000000000000000 ) ) ;
#10491 = DIRECTION ( 'NONE',  ( -0.4678190685372728419, 0.5302313826179317902, 0.7071067811865437980 ) ) ;
#10492 = ORIENTED_EDGE ( 'NONE', *, *, #9113, .F. ) ;
#10493 = DIRECTION ( 'NONE',  ( 0.000000000000000000, -1.000000000000000000, 3.387121092260456770E-15 ) ) ;
#10494 = AXIS2_PLACEMENT_3D ( 'NONE', #2457, #6684, #1383 ) ;
#10495 = VECTOR ( 'NONE', #4961, 1000.000000000000114 ) ;
#10496 = FACE_OUTER_BOUND ( 'NONE', #13008, .T. ) ;
#10497 = CARTESIAN_POINT ( 'NONE',  ( -16.85849676537586461, 27.93104124342158912, 58.27085874777026930 ) ) ;
#10498 = DIRECTION ( 'NONE',  ( 0.000000000000000000, 1.000000000000000000, -0.000000000000000000 ) ) ;
#10499 = VERTEX_POINT ( 'NONE', #1114 ) ;
#10500 = ADVANCED_FACE ( 'NONE', ( #2123, #6365 ), #5377, .F. ) ;
#10501 = ORIENTED_EDGE ( 'NONE', *, *, #5149, .T. ) ;
#10502 = CIRCLE ( 'NONE', #13623, 3.000000000000000000 ) ;
#10503 =( BOUNDED_CURVE ( )  B_SPLINE_CURVE ( 3, ( #11402, #12381, #9240, #3868 ),
 .UNSPECIFIED., .F., .F. ) 
 B_SPLINE_CURVE_WITH_KNOTS ( ( 4, 4 ),
 ( 0.04873315200000170183, 0.9512668479999960569 ),
 .UNSPECIFIED. ) 
 CURVE ( )  GEOMETRIC_REPRESENTATION_ITEM ( )  RATIONAL_B_SPLINE_CURVE ( ( 0.9230982619916300314, 0.4726811441755540133, 0.4726811441755530141, 0.9230982619916260346 ) ) 
 REPRESENTATION_ITEM ( '' )  );
#10504 = CIRCLE ( 'NONE', #4482, 2.000000000000001776 ) ;
#10505 = AXIS2_PLACEMENT_3D ( 'NONE', #12851, #7522, #1911 ) ;
#10506 = EDGE_LOOP ( 'NONE', ( #11781, #13417, #5322, #13279 ) ) ;
#10507 = VERTEX_POINT ( 'NONE', #993 ) ;
#10508 = ADVANCED_FACE ( 'NONE', ( #9655 ), #11136, .F. ) ;
#10509 = ORIENTED_EDGE ( 'NONE', *, *, #8081, .F. ) ;
#10510 = ORIENTED_EDGE ( 'NONE', *, *, #1602, .F. ) ;
#10511 = PLANE ( 'NONE',  #11112 ) ;
#10512 = CARTESIAN_POINT ( 'NONE',  ( 5.999999999999999112, 11.99999999999999822, 7.000000000000000000 ) ) ;
#10513 = DIRECTION ( 'NONE',  ( 0.000000000000000000, 0.000000000000000000, -1.000000000000000000 ) ) ;
#10514 = PLANE ( 'NONE',  #11005 ) ;
#10515 = DIRECTION ( 'NONE',  ( -1.000000000000000000, 0.000000000000000000, 0.000000000000000000 ) ) ;
#10516 = FACE_OUTER_BOUND ( 'NONE', #11958, .T. ) ;
#10517 = PLANE ( 'NONE',  #6689 ) ;
#10518 = AXIS2_PLACEMENT_3D ( 'NONE', #6362, #6565, #8659 ) ;
#10519 = VECTOR ( 'NONE', #1004, 1000.000000000000000 ) ;
#10520 = ITEM_DEFINED_TRANSFORMATION ( 'NONE', 'NONE', #1545,  #6434 ) ;
#10521 = CIRCLE ( 'NONE', #8495, 6.449999999999997513 ) ;
#10522 = ORIENTED_EDGE ( 'NONE', *, *, #1528, .F. ) ;
#10523 = ORIENTED_EDGE ( 'NONE', *, *, #1051, .T. ) ;
#10524 = CYLINDRICAL_SURFACE ( 'NONE', #3277, 2.000000000000001776 ) ;
#10525 = AXIS2_PLACEMENT_3D ( 'NONE', #13080, #1558, #9888 ) ;
#10526 = CARTESIAN_POINT ( 'NONE',  ( 50.38563590245420443, 94.65549801902425031, 23.00000000000000000 ) ) ;
#10527 = AXIS2_PLACEMENT_3D ( 'NONE', #9468, #4159, #8407 ) ;
#10528 = ORIENTED_EDGE ( 'NONE', *, *, #11052, .T. ) ;
#10529 = DIRECTION ( 'NONE',  ( 1.000000000000000000, 0.000000000000000000, 0.000000000000000000 ) ) ;
#10530 = LINE ( 'NONE', #10382, #2419 ) ;
#10531 = CARTESIAN_POINT ( 'NONE',  ( -1.059188295049996231, 27.97290950744599769, 64.35000000000000853 ) ) ;
#10532 = CARTESIAN_POINT ( 'NONE',  ( -16.20671929495594910, 8.873300352462479168, 23.90000000000000213 ) ) ;
#10533 = ORIENTED_EDGE ( 'NONE', *, *, #230, .F. ) ;
#10534 = DIRECTION ( 'NONE',  ( -0.4528443260392610581, -0.8915896008669277339, 0.000000000000000000 ) ) ;
#10535 = DIRECTION ( 'NONE',  ( 0.000000000000000000, 0.000000000000000000, -1.000000000000000000 ) ) ;
#10536 = EDGE_CURVE ( 'NONE', #10337, #5356, #633, .T. ) ;
#10537 = CARTESIAN_POINT ( 'NONE',  ( -1.059188295049996231, -6.027090492554000534, 58.85000000000000142 ) ) ;
#10538 = CARTESIAN_POINT ( 'NONE',  ( -40.05918829504999934, -11.02709049255400053, 0.000000000000000000 ) ) ;
#10539 = CARTESIAN_POINT ( 'NONE',  ( -28.87730642030694739, -7.867426463707978712, 5.250000000000000000 ) ) ;
#10540 = AXIS2_PLACEMENT_3D ( 'NONE', #3011, #12413, #746 ) ;
#10541 = ORIENTED_EDGE ( 'NONE', *, *, #9485, .F. ) ;
#10542 = DIRECTION ( 'NONE',  ( 0.000000000000000000, 0.000000000000000000, -1.000000000000000000 ) ) ;
#10543 = ORIENTED_EDGE ( 'NONE', *, *, #11857, .T. ) ;
#10544 = VERTEX_POINT ( 'NONE', #7520 ) ;
#10545 = CYLINDRICAL_SURFACE ( 'NONE', #11309, 0.5000000000000004441 ) ;
#10546 = VECTOR ( 'NONE', #808, 1000.000000000000000 ) ;
#10547 = DIRECTION ( 'NONE',  ( -0.000000000000000000, -0.000000000000000000, 1.000000000000000000 ) ) ;
#10548 = DIRECTION ( 'NONE',  ( 0.000000000000000000, 0.000000000000000000, 1.000000000000000000 ) ) ;
#10549 = EDGE_CURVE ( 'NONE', #11675, #4278, #8456, .T. ) ;
#10550 = CARTESIAN_POINT ( 'NONE',  ( 134.6356359024541973, 108.9054980190242503, 22.89644660940672694 ) ) ;
#10551 = ADVANCED_FACE ( 'NONE', ( #921 ), #5180, .T. ) ;
#10552 = DIRECTION ( 'NONE',  ( 0.000000000000000000, 0.000000000000000000, 1.000000000000000000 ) ) ;
#10553 = EDGE_CURVE ( 'NONE', #10426, #7735, #9001, .T. ) ;
#10554 = CIRCLE ( 'NONE', #10328, 8.300000000000000711 ) ;
#10555 = CARTESIAN_POINT ( 'NONE',  ( -14.82335591628575777, 30.13379967402607562, 59.67111322632907644 ) ) ;
#10556 = ORIENTED_EDGE ( 'NONE', *, *, #2714, .T. ) ;
#10557 = VERTEX_POINT ( 'NONE', #7869 ) ;
#10558 = ORIENTED_EDGE ( 'NONE', *, *, #9472, .F. ) ;
#10559 = CARTESIAN_POINT ( 'NONE',  ( -12.62505638257885998, 21.67198471784914915, 57.35000000000000142 ) ) ;
#10560 =( NAMED_UNIT ( * ) PLANE_ANGLE_UNIT ( ) SI_UNIT ( $, .RADIAN. ) );
#10561 = CARTESIAN_POINT ( 'NONE',  ( -21.05918829505000289, 10.97290950744599947, 118.8499999999999943 ) ) ;
#10562 = FACE_OUTER_BOUND ( 'NONE', #6353, .T. ) ;
#10563 = DIRECTION ( 'NONE',  ( 0.000000000000000000, 0.000000000000000000, -1.000000000000000000 ) ) ;
#10564 = EDGE_CURVE ( 'NONE', #2075, #1834, #10448, .T. ) ;
#10565 = VECTOR ( 'NONE', #4336, 1000.000000000000000 ) ;
#10566 = CARTESIAN_POINT ( 'NONE',  ( -11.63918829504999941, 10.97290950744599947, 64.85000000000000853 ) ) ;
#10567 = DIRECTION ( 'NONE',  ( 0.000000000000000000, 0.000000000000000000, 1.000000000000000000 ) ) ;
#10568 = EDGE_CURVE ( 'NONE', #642, #1042, #4216, .T. ) ;
#10569 = EDGE_CURVE ( 'NONE', #11868, #2414, #8898, .T. ) ;
#10570 = ORIENTED_EDGE ( 'NONE', *, *, #50, .F. ) ;
#10571 = EDGE_LOOP ( 'NONE', ( #5884, #5547 ) ) ;
#10572 = VERTEX_POINT ( 'NONE', #12148 ) ;
#10573 = EDGE_LOOP ( 'NONE', ( #8557, #4937, #589, #1361, #4310, #11668 ) ) ;
#10574 = CARTESIAN_POINT ( 'NONE',  ( -18.05918829504999934, 10.97290950744599947, 53.85000000000000142 ) ) ;
#10575 = DIRECTION ( 'NONE',  ( 0.000000000000000000, 0.000000000000000000, 1.000000000000000000 ) ) ;
#10576 = EDGE_CURVE ( 'NONE', #2952, #9970, #6824, .T. ) ;
#10577 = ORIENTED_EDGE ( 'NONE', *, *, #8612, .T. ) ;
#10578 = CARTESIAN_POINT ( 'NONE',  ( -21.16117192841894834, 4.865520741507539881, 64.54999999999999716 ) ) ;
#10579 = DIRECTION ( 'NONE',  ( 1.000000000000000000, 0.000000000000000000, 0.000000000000000000 ) ) ;
#10580 = DIRECTION ( 'NONE',  ( -1.000000000000000000, 0.000000000000000000, 0.000000000000000000 ) ) ;
#10581 = CARTESIAN_POINT ( 'NONE',  ( -11.63918829504999941, 10.97290950744599947, 64.85000000000000853 ) ) ;
#10582 = EDGE_CURVE ( 'NONE', #2781, #5561, #9787, .T. ) ;
#10583 = CYLINDRICAL_SURFACE ( 'NONE', #7567, 9.999999999999994671 ) ;
#10584 = ITEM_DEFINED_TRANSFORMATION ( 'NONE', 'NONE', #11138,  #6434 ) ;
#10585 = EDGE_CURVE ( 'NONE', #7731, #4661, #3769, .T. ) ;
#10586 = ORIENTED_EDGE ( 'NONE', *, *, #11520, .F. ) ;
#10587 = CARTESIAN_POINT ( 'NONE',  ( 92.63563590245421153, 99.03908161011133870, 0.000000000000000000 ) ) ;
#10588 = FACE_OUTER_BOUND ( 'NONE', #5723, .T. ) ;
#10589 = CARTESIAN_POINT ( 'NONE',  ( 8.500000000000003553, 2.500000000000000000, -65.00000000000000000 ) ) ;
#10590 = CARTESIAN_POINT ( 'NONE',  ( 44.94629607423404849, 85.78908161011133870, 0.000000000000000000 ) ) ;
#10591 = SURFACE_SIDE_STYLE ('',( #6337 ) ) ;
#10592 = VERTEX_POINT ( 'NONE', #11236 ) ;
#10593 = CARTESIAN_POINT ( 'NONE',  ( 0.000000000000000000, 8.500000000000000000, -13.50000000000000000 ) ) ;
#10594 = CARTESIAN_POINT ( 'NONE',  ( 140.6356359024541973, 103.9054980190242361, 23.00000000000000000 ) ) ;
#10595 = CARTESIAN_POINT ( 'NONE',  ( 142.6356359024541973, 87.03908161011133870, 0.7500000000000006661 ) ) ;
#10596 = EDGE_LOOP ( 'NONE', ( #8551, #8599, #11915, #9357 ) ) ;
#10597 = LINE ( 'NONE', #5416, #7550 ) ;
#10598 = EDGE_CURVE ( 'NONE', #1636, #803, #1659, .T. ) ;
#10599 = EDGE_CURVE ( 'NONE', #7458, #9458, #7768, .T. ) ;
#10600 = VERTEX_POINT ( 'NONE', #1516 ) ;
#10601 = AXIS2_PLACEMENT_3D ( 'NONE', #4769, #5797, #5659 ) ;
#10602 = EDGE_LOOP ( 'NONE', ( #9287, #5118, #9329, #9395, #815, #9416 ) ) ;
#10603 = FACE_BOUND ( 'NONE', #3560, .T. ) ;
#10604 = ORIENTED_EDGE ( 'NONE', *, *, #2363, .T. ) ;
#10605 = VERTEX_POINT ( 'NONE', #11161 ) ;
#10606 = ORIENTED_EDGE ( 'NONE', *, *, #1225, .T. ) ;
#10607 = ORIENTED_EDGE ( 'NONE', *, *, #3803, .F. ) ;
#10608 = CARTESIAN_POINT ( 'NONE',  ( -13.43623923775013651, 8.383794209755873084, 68.55139394072084258 ) ) ;
#10609 = CARTESIAN_POINT ( 'NONE',  ( -18.05918829504999934, 10.97290950744599947, 17.25000000000000000 ) ) ;
#10610 = DIRECTION ( 'NONE',  ( 0.000000000000000000, 0.000000000000000000, 1.000000000000000000 ) ) ;
#10611 = DIRECTION ( 'NONE',  ( 0.000000000000000000, -1.000000000000000000, 0.000000000000000000 ) ) ;
#10612 = AXIS2_PLACEMENT_3D ( 'NONE', #11586, #2954, #10468 ) ;
#10613 = CARTESIAN_POINT ( 'NONE',  ( 12.00000000000000000, -2.499999999999999556, -65.00000000000000000 ) ) ;
#10614 = UNCERTAINTY_MEASURE_WITH_UNIT (LENGTH_MEASURE( 1.000000000000000082E-05 ), #5489, 'distance_accuracy_value', 'NONE');
#10615 = EDGE_CURVE ( 'NONE', #821, #11588, #12919, .T. ) ;
#10616 = ORIENTED_EDGE ( 'NONE', *, *, #7451, .F. ) ;
#10617 = EDGE_CURVE ( 'NONE', #1687, #2014, #13342, .T. ) ;
#10618 = AXIS2_PLACEMENT_3D ( 'NONE', #10048, #4737, #3556 ) ;
#10619 = CARTESIAN_POINT ( 'NONE',  ( -16.50344191708178343, 30.30811942209297882, 53.37097390537915942 ) ) ;
#10620 = VERTEX_POINT ( 'NONE', #12074 ) ;
#10621 = EDGE_LOOP ( 'NONE', ( #1994, #6315 ) ) ;
#10622 = DIRECTION ( 'NONE',  ( 0.000000000000000000, 0.000000000000000000, -1.000000000000000000 ) ) ;
#10623 = DIRECTION ( 'NONE',  ( 1.000000000000000000, 0.000000000000000000, 0.000000000000000000 ) ) ;
#10624 = FACE_OUTER_BOUND ( 'NONE', #6089, .T. ) ;
#10625 = ORIENTED_EDGE ( 'NONE', *, *, #3002, .T. ) ;
#10626 = CARTESIAN_POINT ( 'NONE',  ( 7.640422211807137209, 16.89844320975774750, -3.000000000000000000 ) ) ;
#10627 = DIRECTION ( 'NONE',  ( 0.000000000000000000, 0.000000000000000000, 1.000000000000000000 ) ) ;
#10628 = DIRECTION ( 'NONE',  ( 1.000000000000000000, 0.000000000000000000, 0.000000000000000000 ) ) ;
#10629 = CIRCLE ( 'NONE', #8396, 6.345833333000001630 ) ;
#10630 = CARTESIAN_POINT ( 'NONE',  ( -18.05918829504999934, 10.97290950744599947, 27.30000000000000071 ) ) ;
#10631 = ORIENTED_EDGE ( 'NONE', *, *, #2732, .T. ) ;
#10632 = EDGE_CURVE ( 'NONE', #7171, #10095, #4804, .T. ) ;
#10633 = CARTESIAN_POINT ( 'NONE',  ( -18.05918829504999934, 10.97290950744599947, 61.72253826518770836 ) ) ;
#10634 = ORIENTED_EDGE ( 'NONE', *, *, #9810, .T. ) ;
#10635 = ORIENTED_EDGE ( 'NONE', *, *, #12911, .T. ) ;
#10636 = ORIENTED_EDGE ( 'NONE', *, *, #12852, .F. ) ;
#10637 = AXIS2_PLACEMENT_3D ( 'NONE', #12303, #8026, #11177 ) ;
#10638 = ORIENTED_EDGE ( 'NONE', *, *, #8061, .F. ) ;
#10639 = CYLINDRICAL_SURFACE ( 'NONE', #9553, 1.999999999999991340 ) ;
#10640 = CARTESIAN_POINT ( 'NONE',  ( -40.05918829505000645, 32.97290950744599769, 10.00000000000000000 ) ) ;
#10641 = EDGE_CURVE ( 'NONE', #7297, #12897, #3529, .T. ) ;
#10642 = ORIENTED_EDGE ( 'NONE', *, *, #926, .T. ) ;
#10643 = DIRECTION ( 'NONE',  ( -1.000000000000000000, 0.000000000000000000, 0.000000000000000000 ) ) ;
#10644 = CARTESIAN_POINT ( 'NONE',  ( 8.500000000000001776, 2.000000000000000000, -65.00000000000000000 ) ) ;
#10645 = CYLINDRICAL_SURFACE ( 'NONE', #8197, 0.2500000000000002220 ) ;
#10646 = DIRECTION ( 'NONE',  ( -0.6615960714621568206, 0.7498604124941127269, 0.000000000000000000 ) ) ;
#10647 = DIRECTION ( 'NONE',  ( -1.000000000000000000, 0.000000000000000000, 0.000000000000000000 ) ) ;
#10648 = CONICAL_SURFACE ( 'NONE', #12875, 5.500000000000002665, 0.7853981633974433940 ) ;
#10649 = EDGE_CURVE ( 'NONE', #6783, #5985, #10031, .T. ) ;
#10650 = ORIENTED_EDGE ( 'NONE', *, *, #279, .F. ) ;
#10651 = DIRECTION ( 'NONE',  ( 0.000000000000000000, 0.000000000000000000, 1.000000000000000000 ) ) ;
#10652 = ORIENTED_EDGE ( 'NONE', *, *, #10315, .T. ) ;
#10653 = AXIS2_PLACEMENT_3D ( 'NONE', #11285, #12342, #4993 ) ;
#10654 = CARTESIAN_POINT ( 'NONE',  ( 8.500000000000001776, 2.000000000000000000, 0.000000000000000000 ) ) ;
#10655 = VECTOR ( 'NONE', #10951, 1000.000000000000000 ) ;
#10656 = DIRECTION ( 'NONE',  ( 0.000000000000000000, 0.000000000000000000, -1.000000000000000000 ) ) ;
#10657 = CARTESIAN_POINT ( 'NONE',  ( -24.37001676333060018, -4.028726038184999858, 62.14999999999999858 ) ) ;
#10658 = ADVANCED_FACE ( 'NONE', ( #5843 ), #8012, .T. ) ;
#10659 = CARTESIAN_POINT ( 'NONE',  ( -20.28116495117919271, 30.25376030680740769, 53.80727490026070825 ) ) ;
#10660 = DIRECTION ( 'NONE',  ( 1.000000000000000000, -0.000000000000000000, 0.000000000000000000 ) ) ;
#10661 = DIRECTION ( 'NONE',  ( 0.000000000000000000, 0.000000000000000000, 1.000000000000000000 ) ) ;
#10662 = CARTESIAN_POINT ( 'NONE',  ( -22.58763155544259860, 2.057013498776719906, 64.85000000000000853 ) ) ;
#10663 = CARTESIAN_POINT ( 'NONE',  ( 4.000000000000001776, -4.336808689942017736E-16, -65.00000000000000000 ) ) ;
#10664 = CARTESIAN_POINT ( 'NONE',  ( -36.55918829504999934, 10.97290950744599947, 12.50000000000000000 ) ) ;
#10665 = ORIENTED_EDGE ( 'NONE', *, *, #6939, .T. ) ;
#10666 = CIRCLE ( 'NONE', #4649, 17.66282263685195275 ) ;
#10667 = CIRCLE ( 'NONE', #837, 2.000000000000001776 ) ;
#10668 = AXIS2_PLACEMENT_3D ( 'NONE', #6692, #5568, #9858 ) ;
#10669 = ADVANCED_FACE ( 'NONE', ( #11035 ), #608, .F. ) ;
#10670 = CIRCLE ( 'NONE', #4867, 1.500000000000001332 ) ;
#10671 = ORIENTED_EDGE ( 'NONE', *, *, #8464, .T. ) ;
#10672 = ORIENTED_EDGE ( 'NONE', *, *, #3227, .F. ) ;
#10673 = DIRECTION ( 'NONE',  ( -1.000000000000000000, 0.000000000000000000, 0.000000000000000000 ) ) ;
#10674 = EDGE_LOOP ( 'NONE', ( #2563, #5423, #7231, #11690 ) ) ;
#10675 = ORIENTED_EDGE ( 'NONE', *, *, #2542, .T. ) ;
#10676 = EDGE_LOOP ( 'NONE', ( #2932, #5537, #1396, #723, #9204 ) ) ;
#10677 = DIRECTION ( 'NONE',  ( 0.000000000000000000, 0.000000000000000000, 1.000000000000000000 ) ) ;
#10678 = EDGE_CURVE ( 'NONE', #3389, #10425, #2737, .T. ) ;
#10679 = CARTESIAN_POINT ( 'NONE',  ( 12.00000000000000000, -2.499999999999999556, 0.000000000000000000 ) ) ;
#10680 = ORIENTED_EDGE ( 'NONE', *, *, #12457, .T. ) ;
#10681 = DIRECTION ( 'NONE',  ( -1.000000000000000000, 0.000000000000000000, 0.000000000000000000 ) ) ;
#10682 = ORIENTED_EDGE ( 'NONE', *, *, #2034, .T. ) ;
#10683 = CIRCLE ( 'NONE', #11778, 1.999999999999994893 ) ;
#10684 = AXIS2_PLACEMENT_3D ( 'NONE', #1727, #678, #9341 ) ;
#10685 = DIRECTION ( 'NONE',  ( 0.000000000000000000, 0.000000000000000000, 1.000000000000000000 ) ) ;
#10686 = AXIS2_PLACEMENT_3D ( 'NONE', #8590, #10563, #12846 ) ;
#10687 = CARTESIAN_POINT ( 'NONE',  ( -28.87730642030695094, 29.81324547859994922, 17.25000000000000000 ) ) ;
#10688 = CIRCLE ( 'NONE', #11813, 2.000000000000001776 ) ;
#10689 = ORIENTED_EDGE ( 'NONE', *, *, #2987, .T. ) ;
#10690 = AXIS2_PLACEMENT_3D ( 'NONE', #13316, #2532, #9719 ) ;
#10691 = CARTESIAN_POINT ( 'NONE',  ( -15.48247209720144113, 30.21696533453561173, 54.13423996167696828 ) ) ;
#10692 = ORIENTED_EDGE ( 'NONE', *, *, #2138, .T. ) ;
#10693 = VERTEX_POINT ( 'NONE', #9136 ) ;
#10694 = CARTESIAN_POINT ( 'NONE',  ( -7.241070169793076161, -7.867426463707975159, 17.25000000000000000 ) ) ;
#10695 = DIRECTION ( 'NONE',  ( 0.000000000000000000, 0.000000000000000000, -1.000000000000000000 ) ) ;
#10696 = LINE ( 'NONE', #4348, #12080 ) ;
#10697 = DIRECTION ( 'NONE',  ( -0.7071067811865474617, -0.7071067811865474617, 0.000000000000000000 ) ) ;
#10698 = CARTESIAN_POINT ( 'NONE',  ( -8.814269998155332075, 15.06602133594271820, 7.000000000000000000 ) ) ;
#10699 = CARTESIAN_POINT ( 'NONE',  ( -3.499999999999998224, 2.499999999999999556, -65.00000000000000000 ) ) ;
#10700 = EDGE_CURVE ( 'NONE', #4490, #13747, #405, .T. ) ;
#10701 = DIRECTION ( 'NONE',  ( 0.000000000000000000, 0.000000000000000000, -1.000000000000000000 ) ) ;
#10702 = AXIS2_PLACEMENT_3D ( 'NONE', #9385, #13496, #3938 ) ;
#10703 = AXIS2_PLACEMENT_3D ( 'NONE', #870, #797, #12270 ) ;
#10704 = VERTEX_POINT ( 'NONE', #7360 ) ;
#10705 = ORIENTED_EDGE ( 'NONE', *, *, #6820, .F. ) ;
#10706 = FACE_OUTER_BOUND ( 'NONE', #9219, .T. ) ;
#10707 = VERTEX_POINT ( 'NONE', #9274 ) ;
#10708 = ORIENTED_EDGE ( 'NONE', *, *, #2342, .F. ) ;
#10709 = VECTOR ( 'NONE', #1895, 1000.000000000000000 ) ;
#10710 = PRODUCT_DEFINITION_SHAPE ( 'NONE', 'NONE',  #13810 ) ;
#10711 = EDGE_CURVE ( 'NONE', #12138, #10605, #11326, .T. ) ;
#10712 = TOROIDAL_SURFACE ( 'NONE', #4253, 10.75000000000000000, 0.7500000000000000000 ) ;
#10713 = CARTESIAN_POINT ( 'NONE',  ( -22.71804201037815218, -4.525318844826149878, 62.14999999999999858 ) ) ;
#10714 = CARTESIAN_POINT ( 'NONE',  ( 123.1053058165639555, 68.56941169600116837, 20.00000000000000000 ) ) ;
#10715 = ORIENTED_EDGE ( 'NONE', *, *, #7658, .F. ) ;
#10716 = DIRECTION ( 'NONE',  ( 0.000000000000000000, 1.000000000000000000, 0.000000000000000000 ) ) ;
#10717 = CARTESIAN_POINT ( 'NONE',  ( -19.46048213834016494, 26.91143339763804221, 56.81345751610173522 ) ) ;
#10718 = CARTESIAN_POINT ( 'NONE',  ( -13.05918829504999756, 10.97290950744599947, 68.84999999999999432 ) ) ;
#10719 = DIRECTION ( 'NONE',  ( 0.000000000000000000, 0.000000000000000000, -1.000000000000000000 ) ) ;
#10720 = ADVANCED_FACE ( 'NONE', ( #8149 ), #13726, .F. ) ;
#10721 = DIRECTION ( 'NONE',  ( 0.000000000000000000, 0.000000000000000000, 1.000000000000000000 ) ) ;
#10722 = VERTEX_POINT ( 'NONE', #12560 ) ;
#10723 = AXIS2_PLACEMENT_3D ( 'NONE', #9915, #9205, #2862 ) ;
#10724 = AXIS2_PLACEMENT_3D ( 'NONE', #3366, #7597, #11883 ) ;
#10725 = VECTOR ( 'NONE', #9092, 1000.000000000000000 ) ;
#10726 = ORIENTED_EDGE ( 'NONE', *, *, #13277, .T. ) ;
#10727 = CARTESIAN_POINT ( 'NONE',  ( -10.47404583389237942, 25.90703532196704728, 61.85000000000000142 ) ) ;
#10728 = DIRECTION ( 'NONE',  ( 0.000000000000000000, 0.000000000000000000, 1.000000000000000000 ) ) ;
#10729 = CARTESIAN_POINT ( 'NONE',  ( 141.8856359024541973, 85.03908161011133870, 0.7500000000000006661 ) ) ;
#10730 = DIRECTION ( 'NONE',  ( 0.000000000000000000, 0.000000000000000000, -1.000000000000000000 ) ) ;
#10731 = CARTESIAN_POINT ( 'NONE',  ( -18.52354985390699937, 30.35570588519016155, 53.02278649370575181 ) ) ;
#10732 = AXIS2_PLACEMENT_3D ( 'NONE', #191, #3489, #4391 ) ;
#10733 = DIRECTION ( 'NONE',  ( 0.000000000000000000, 0.000000000000000000, -1.000000000000000000 ) ) ;
#10734 = ORIENTED_EDGE ( 'NONE', *, *, #5610, .F. ) ;
#10735 = FACE_OUTER_BOUND ( 'NONE', #4203, .T. ) ;
#10736 = AXIS2_PLACEMENT_3D ( 'NONE', #5475, #5343, #10953 ) ;
#10737 = DIRECTION ( 'NONE',  ( -1.000000000000000000, 0.000000000000000000, -0.000000000000000000 ) ) ;
#10738 = FACE_OUTER_BOUND ( 'NONE', #3345, .T. ) ;
#10739 = EDGE_CURVE ( 'NONE', #6209, #1934, #12474, .T. ) ;
#10740 = CARTESIAN_POINT ( 'NONE',  ( 92.63563590245421153, 99.03908161011133870, 19.25000000000000000 ) ) ;
#10741 = SHAPE_REPRESENTATION_RELATIONSHIP ( 'NONE' , 'NONE' ,  #12309, #5398 ) ;
#10742 = ADVANCED_FACE ( 'NONE', ( #2942 ), #7091, .F. ) ;
#10743 = EDGE_CURVE ( 'NONE', #13747, #1567, #2691, .T. ) ;
#10744 = EDGE_CURVE ( 'NONE', #3595, #182, #2329, .T. ) ;
#10745 = CIRCLE ( 'NONE', #12531, 1.999999999999994893 ) ;
#10746 = AXIS2_PLACEMENT_3D ( 'NONE', #12268, #12194, #8838 ) ;
#10747 = FACE_BOUND ( 'NONE', #13345, .T. ) ;
#10748 = EDGE_LOOP ( 'NONE', ( #2386, #7893 ) ) ;
#10749 = VERTEX_POINT ( 'NONE', #8218 ) ;
#10750 = VERTEX_POINT ( 'NONE', #1806 ) ;
#10751 = LINE ( 'NONE', #8787, #3517 ) ;
#10752 = CARTESIAN_POINT ( 'NONE',  ( -8.499999999999998224, 2.000000000000000000, -65.00000000000000000 ) ) ;
#10753 = CARTESIAN_POINT ( 'NONE',  ( -18.05918829504999934, 10.00028003023991907, 62.14999999999999858 ) ) ;
#10754 = FACE_OUTER_BOUND ( 'NONE', #1356, .T. ) ;
#10755 = DIRECTION ( 'NONE',  ( -0.000000000000000000, 1.000000000000000000, -0.000000000000000000 ) ) ;
#10756 = EDGE_CURVE ( 'NONE', #1633, #7102, #648, .T. ) ;
#10757 = VECTOR ( 'NONE', #541, 1000.000000000000000 ) ;
#10758 = DIRECTION ( 'NONE',  ( 0.000000000000000000, 0.000000000000000000, -1.000000000000000000 ) ) ;
#10759 = FACE_OUTER_BOUND ( 'NONE', #11605, .T. ) ;
#10760 = EDGE_CURVE ( 'NONE', #3796, #8205, #1733, .T. ) ;
#10761 = ORIENTED_EDGE ( 'NONE', *, *, #7880, .T. ) ;
#10762 = PRESENTATION_LAYER_ASSIGNMENT (  '', '', ( #7617 ) ) ;
#10763 = CARTESIAN_POINT ( 'NONE',  ( -15.83390592052727186, 30.25344248475043685, 53.80997457889011315 ) ) ;
#10764 = ORIENTED_EDGE ( 'NONE', *, *, #5349, .T. ) ;
#10765 = ORIENTED_EDGE ( 'NONE', *, *, #4240, .T. ) ;
#10766 = FILL_AREA_STYLE ('',( #5501 ) ) ;
#10767 = CARTESIAN_POINT ( 'NONE',  ( 2.262399129208279902, 22.44393519180574970, 5.250000000000000000 ) ) ;
#10768 =( NAMED_UNIT ( * ) PLANE_ANGLE_UNIT ( ) SI_UNIT ( $, .RADIAN. ) );
#10769 = LINE ( 'NONE', #9791, #645 ) ;
#10770 = DIRECTION ( 'NONE',  ( 0.7071067811865567876, 0.7071067811865382469, 0.000000000000000000 ) ) ;
#10771 = CARTESIAN_POINT ( 'NONE',  ( -1.627166789049998563, 2.756898754446010180, 63.36264408499989287 ) ) ;
#10772 = DIRECTION ( 'NONE',  ( -1.000000000000000000, 0.000000000000000000, 0.000000000000000000 ) ) ;
#10773 = AXIS2_PLACEMENT_3D ( 'NONE', #3814, #9257, #3950 ) ;
#10774 = PRODUCT ( 'Rotary Faceplate', 'Rotary Faceplate', '', ( #11358 ) ) ;
#10775 = EDGE_CURVE ( 'NONE', #703, #223, #962, .T. ) ;
#10776 = ORIENTED_EDGE ( 'NONE', *, *, #11900, .T. ) ;
#10777 = ORIENTED_EDGE ( 'NONE', *, *, #9864, .T. ) ;
#10778 = VERTEX_POINT ( 'NONE', #5211 ) ;
#10779 = CARTESIAN_POINT ( 'NONE',  ( -5.173045190668890569, -15.68519459986890041, 17.25000000000000000 ) ) ;
#10780 = EDGE_LOOP ( 'NONE', ( #4529, #2980, #6754, #11000 ) ) ;
#10781 = VERTEX_POINT ( 'NONE', #11437 ) ;
#10782 = EDGE_LOOP ( 'NONE', ( #362, #8815, #8400, #1340 ) ) ;
#10783 = CIRCLE ( 'NONE', #11897, 4.250000000000000000 ) ;
#10784 = DIRECTION ( 'NONE',  ( 1.000000000000000000, 0.000000000000000000, 0.000000000000000000 ) ) ;
#10785 = CARTESIAN_POINT ( 'NONE',  ( 142.6356359024541973, 85.03908161011133870, 20.00000000000000000 ) ) ;
#10786 = ORIENTED_EDGE ( 'NONE', *, *, #12832, .T. ) ;
#10787 = CARTESIAN_POINT ( 'NONE',  ( -18.05918829504999934, 10.97290950744599947, 61.65955166399999854 ) ) ;
#10788 = CARTESIAN_POINT ( 'NONE',  ( -17.22489654692306971, 26.95114159751178562, 56.10333731137770741 ) ) ;
#10789 = CARTESIAN_POINT ( 'NONE',  ( 141.8856359024541973, 110.7284214383315089, 0.000000000000000000 ) ) ;
#10790 = CARTESIAN_POINT ( 'NONE',  ( -18.05918829504999934, 10.97290950744599947, 60.60999999999999943 ) ) ;
#10791 = CARTESIAN_POINT ( 'NONE',  ( -18.05918829504999934, 10.97290950744599947, 63.45000000000000284 ) ) ;
#10792 = ITEM_DEFINED_TRANSFORMATION ( 'NONE', 'NONE', #11796,  #6434 ) ;
#10793 = CIRCLE ( 'NONE', #2559, 3.000000000000002665 ) ;
#10794 = ADVANCED_FACE ( 'NONE', ( #2027 ), #10385, .T. ) ;
#10795 = EDGE_CURVE ( 'NONE', #3923, #7555, #5952, .T. ) ;
#10796 = ADVANCED_FACE ( 'NONE', ( #7288 ), #5293, .F. ) ;
#10797 = ORIENTED_EDGE ( 'NONE', *, *, #10553, .F. ) ;
#10798 = VERTEX_POINT ( 'NONE', #5145 ) ;
#10799 = ADVANCED_FACE ( 'NONE', ( #9422 ), #3777, .T. ) ;
#10800 = DIRECTION ( 'NONE',  ( 0.000000000000000000, 0.000000000000000000, -1.000000000000000000 ) ) ;
#10801 = DIRECTION ( 'NONE',  ( -1.000000000000000000, 0.000000000000000000, 0.000000000000000000 ) ) ;
#10802 = EDGE_CURVE ( 'NONE', #6080, #1109, #13668, .T. ) ;
#10803 = ORIENTED_EDGE ( 'NONE', *, *, #4424, .F. ) ;
#10804 = CARTESIAN_POINT ( 'NONE',  ( 116.7775623211734342, 112.2890816101113387, 0.7500000000000006661 ) ) ;
#10805 = CARTESIAN_POINT ( 'NONE',  ( -0.04028432657539327000, 4.500000000000000000, 18.54539866546729243 ) ) ;
#10806 = DIRECTION ( 'NONE',  ( 0.000000000000000000, 0.000000000000000000, -1.000000000000000000 ) ) ;
#10807 = EDGE_LOOP ( 'NONE', ( #9143, #11828, #12102, #13621 ) ) ;
#10808 = CARTESIAN_POINT ( 'NONE',  ( -18.05918829505001355, 18.58149382944599992, 61.98378871700002435 ) ) ;
#10809 = CARTESIAN_POINT ( 'NONE',  ( 134.8856359024541973, 0.000000000000000000, 22.75000000000000000 ) ) ;
#10810 = CARTESIAN_POINT ( 'NONE',  ( -18.05918829488915023, 18.13901823688300396, 61.72253826514069175 ) ) ;
#10811 = DIRECTION ( 'NONE',  ( 1.000000000000000000, 0.000000000000000000, 0.000000000000000000 ) ) ;
#10812 = EDGE_CURVE ( 'NONE', #7807, #6311, #2303, .T. ) ;
#10813 = VERTEX_POINT ( 'NONE', #5412 ) ;
#10814 = FACE_OUTER_BOUND ( 'NONE', #8569, .T. ) ;
#10815 = ORIENTED_EDGE ( 'NONE', *, *, #7031, .T. ) ;
#10816 = CARTESIAN_POINT ( 'NONE',  ( 134.6356359024541973, 89.90549801902423610, 20.00000000000000000 ) ) ;
#10817 = CARTESIAN_POINT ( 'NONE',  ( -1.059188295049996231, -6.027090492554000534, 68.85549045786049760 ) ) ;
#10818 = ADVANCED_FACE ( 'NONE', ( #12886 ), #7531, .F. ) ;
#10819 = CYLINDRICAL_SURFACE ( 'NONE', #1815, 0.5000000000000004441 ) ;
#10820 = LINE ( 'NONE', #7377, #6511 ) ;
#10821 = DIRECTION ( 'NONE',  ( -0.000000000000000000, 1.000000000000000000, -0.000000000000000000 ) ) ;
#10822 = DIRECTION ( 'NONE',  ( 0.000000000000000000, -1.000000000000000000, 2.732534507816519619E-15 ) ) ;
#10823 = DIRECTION ( 'NONE',  ( 0.6615960714621565986, -0.7498604124941128379, 0.000000000000000000 ) ) ;
#10824 = EDGE_CURVE ( 'NONE', #5798, #9556, #1316, .T. ) ;
#10825 = DIRECTION ( 'NONE',  ( 0.000000000000000000, 0.000000000000000000, 1.000000000000000000 ) ) ;
#10826 = AXIS2_PLACEMENT_3D ( 'NONE', #4823, #3711, #12231 ) ;
#10827 = EDGE_CURVE ( 'NONE', #9556, #9938, #8905, .T. ) ;
#10828 = ADVANCED_FACE ( 'NONE', ( #12821 ), #3208, .F. ) ;
#10829 = CARTESIAN_POINT ( 'NONE',  ( -15.39172992069172174, 30.20666037739588461, 54.23161053768875917 ) ) ;
#10830 = EDGE_LOOP ( 'NONE', ( #922, #3251, #2956, #5218 ) ) ;
#10831 = CARTESIAN_POINT ( 'NONE',  ( -7.241070169793063727, -7.867426463707971607, 83.57661607529820458 ) ) ;
#10832 = CIRCLE ( 'NONE', #8822, 3.449999999999999734 ) ;
#10833 = ADVANCED_FACE ( 'NONE', ( #13791 ), #11583, .F. ) ;
#10834 = LINE ( 'NONE', #11949, #7138 ) ;
#10835 = MECHANICAL_DESIGN_GEOMETRIC_PRESENTATION_REPRESENTATION (  '', ( #9212 ), #464 ) ;
#10836 = CARTESIAN_POINT ( 'NONE',  ( 44.63563590245421864, 85.03908161011133870, 19.25000000000000000 ) ) ;
#10837 = EDGE_LOOP ( 'NONE', ( #9241, #13494, #12461, #8253 ) ) ;
#10838 = DIRECTION ( 'NONE',  ( 1.000000000000000000, 0.000000000000000000, 0.000000000000000000 ) ) ;
#10839 = EDGE_CURVE ( 'NONE', #9550, #5017, #430, .T. ) ;
#10840 = CARTESIAN_POINT ( 'NONE',  ( -18.05918829504999934, 10.97290950744599947, 57.54999999999999716 ) ) ;
#10841 = DIRECTION ( 'NONE',  ( 1.000000000000000000, 0.000000000000000000, 0.000000000000000000 ) ) ;
#10842 = VECTOR ( 'NONE', #3629, 1000.000000000000000 ) ;
#10843 = VERTEX_POINT ( 'NONE', #9835 ) ;
#10844 = ORIENTED_EDGE ( 'NONE', *, *, #2635, .T. ) ;
#10845 = ORIENTED_EDGE ( 'NONE', *, *, #8592, .T. ) ;
#10846 = EDGE_CURVE ( 'NONE', #6848, #10557, #1776, .T. ) ;
#10847 = VERTEX_POINT ( 'NONE', #7703 ) ;
#10848 = CYLINDRICAL_SURFACE ( 'NONE', #9260, 0.7499999999999924505 ) ;
#10849 = EDGE_LOOP ( 'NONE', ( #7971, #9199, #6021, #12700, #3340, #13421, #13347, #3959, #6147 ) ) ;
#10850 = EDGE_LOOP ( 'NONE', ( #4055, #7615, #3304, #3787 ) ) ;
#10851 = ORIENTED_EDGE ( 'NONE', *, *, #12294, .F. ) ;
#10852 = CARTESIAN_POINT ( 'NONE',  ( -7.499999999999996447, -1.762812401309176307E-15, -65.00000000000000000 ) ) ;
#10853 = DIRECTION ( 'NONE',  ( -0.000000000000000000, 1.000000000000000000, -0.000000000000000000 ) ) ;
#10854 = VERTEX_POINT ( 'NONE', #2230 ) ;
#10855 = VECTOR ( 'NONE', #10988, 1000.000000000000227 ) ;
#10856 = EDGE_CURVE ( 'NONE', #10507, #13375, #8558, .T. ) ;
#10857 = DIRECTION ( 'NONE',  ( 0.000000000000000000, -1.000000000000000000, 0.000000000000000000 ) ) ;
#10858 = CARTESIAN_POINT ( 'NONE',  ( -16.80552491324057485, 26.92504221762977679, 56.52280737812468203 ) ) ;
#10859 = CARTESIAN_POINT ( 'NONE',  ( -34.68447646404997897, 2.660265422446006500, 63.26601075299999621 ) ) ;
#10860 = DIRECTION ( 'NONE',  ( 0.000000000000000000, 0.000000000000000000, -1.000000000000000000 ) ) ;
#10861 = DIRECTION ( 'NONE',  ( 0.000000000000000000, 0.000000000000000000, -1.000000000000000000 ) ) ;
#10862 = ORIENTED_EDGE ( 'NONE', *, *, #5121, .T. ) ;
#10863 = VERTEX_POINT ( 'NONE', #10593 ) ;
#10864 = CIRCLE ( 'NONE', #3508, 2.700000000000000178 ) ;
#10865 = ORIENTED_EDGE ( 'NONE', *, *, #3131, .T. ) ;
#10866 = ORIENTED_EDGE ( 'NONE', *, *, #4865, .T. ) ;
#10867 = LINE ( 'NONE', #1568, #3065 ) ;
#10868 = CARTESIAN_POINT ( 'NONE',  ( 62.16596598834446752, 129.5087515242215090, 20.00000000000000000 ) ) ;
#10869 = ORIENTED_EDGE ( 'NONE', *, *, #9622, .T. ) ;
#10870 = DIRECTION ( 'NONE',  ( 0.6615960714621568206, -0.7498604124941127269, 0.000000000000000000 ) ) ;
#10871 = DIRECTION ( 'NONE',  ( 0.000000000000000000, 0.000000000000000000, -1.000000000000000000 ) ) ;
#10872 = DIRECTION ( 'NONE',  ( 1.000000000000000000, 0.000000000000000000, 0.000000000000000000 ) ) ;
#10873 = LINE ( 'NONE', #1218, #13671 ) ;
#10874 = DIRECTION ( 'NONE',  ( 0.000000000000000000, 0.000000000000000000, 1.000000000000000000 ) ) ;
#10875 = FACE_OUTER_BOUND ( 'NONE', #3824, .T. ) ;
#10876 = CARTESIAN_POINT ( 'NONE',  ( -2.059188295050000228, 10.97290950744599947, 56.84999999999999432 ) ) ;
#10877 = CIRCLE ( 'NONE', #4845, 5.000000000000000888 ) ;
#10878 = CARTESIAN_POINT ( 'NONE',  ( -25.22529702413155306, 10.97290950744599947, 61.72253826518770836 ) ) ;
#10879 =( LENGTH_UNIT ( ) NAMED_UNIT ( * ) SI_UNIT ( .MILLI., .METRE. ) );
#10880 = ADVANCED_FACE ( 'NONE', ( #9546 ), #4244, .T. ) ;
#10881 = VECTOR ( 'NONE', #1643, 1000.000000000000000 ) ;
#10882 = ORIENTED_EDGE ( 'NONE', *, *, #11933, .F. ) ;
#10883 = ORIENTED_EDGE ( 'NONE', *, *, #11990, .T. ) ;
#10884 = VECTOR ( 'NONE', #10036, 1000.000000000000000 ) ;
#10885 = PLANE ( 'NONE',  #1919 ) ;
#10886 = EDGE_LOOP ( 'NONE', ( #4228, #4474, #10359, #13617 ) ) ;
#10887 = CARTESIAN_POINT ( 'NONE',  ( 79.82136590429890077, 114.1051029460540605, 10.00000000000000000 ) ) ;
#10888 = DIRECTION ( 'NONE',  ( 1.000000000000000000, 0.000000000000000000, 0.000000000000000000 ) ) ;
#10889 = DIRECTION ( 'NONE',  ( 0.000000000000000000, 0.000000000000000000, -1.000000000000000000 ) ) ;
#10890 = CYLINDRICAL_SURFACE ( 'NONE', #242, 6.000000000000005329 ) ;
#10891 = CARTESIAN_POINT ( 'NONE',  ( -38.05918829505000645, -6.027090492554000534, 0.000000000000000000 ) ) ;
#10892 = DIRECTION ( 'NONE',  ( -0.6615960714621564875, 0.7498604124941129490, 0.000000000000000000 ) ) ;
#10893 = DIRECTION ( 'NONE',  ( 1.000000000000000000, 0.000000000000000000, 0.000000000000000000 ) ) ;
#10894 = CARTESIAN_POINT ( 'NONE',  ( 142.6356359024541973, 111.0390816101113245, 20.00000000000000000 ) ) ;
#10895 = DIRECTION ( 'NONE',  ( -0.4528443260392611136, -0.8915896008669277339, 0.000000000000000000 ) ) ;
#10896 = VECTOR ( 'NONE', #3163, 1000.000000000000000 ) ;
#10897 = AXIS2_PLACEMENT_3D ( 'NONE', #7993, #10111, #12266 ) ;
#10898 = EDGE_CURVE ( 'NONE', #12210, #11722, #11713, .T. ) ;
#10899 = CIRCLE ( 'NONE', #2887, 4.250000000000000000 ) ;
#10900 = ORIENTED_EDGE ( 'NONE', *, *, #13366, .T. ) ;
#10901 = CARTESIAN_POINT ( 'NONE',  ( -17.79660873271074095, 30.36027202460864416, 52.99086025162979752 ) ) ;
#10902 = VECTOR ( 'NONE', #4881, 1000.000000000000000 ) ;
#10903 = ORIENTED_EDGE ( 'NONE', *, *, #4829, .T. ) ;
#10904 = AXIS2_PLACEMENT_3D ( 'NONE', #196, #9704, #7437 ) ;
#10905 = VERTEX_POINT ( 'NONE', #4318 ) ;
#10906 = DIRECTION ( 'NONE',  ( 1.000000000000000000, 0.000000000000000000, 0.000000000000000000 ) ) ;
#10907 = CIRCLE ( 'NONE', #6882, 24.92993838181874722 ) ;
#10908 = LINE ( 'NONE', #8586, #12936 ) ;
#10909 = ORIENTED_EDGE ( 'NONE', *, *, #12866, .T. ) ;
#10910 = DIRECTION ( 'NONE',  ( 1.000000000000000000, 0.000000000000000000, -0.000000000000000000 ) ) ;
#10911 = DIRECTION ( 'NONE',  ( 1.000000000000000000, -0.000000000000000000, 0.000000000000000000 ) ) ;
#10912 = EDGE_CURVE ( 'NONE', #3167, #13219, #9125, .T. ) ;
#10913 = FACE_BOUND ( 'NONE', #2845, .T. ) ;
#10914 = AXIS2_PLACEMENT_3D ( 'NONE', #10790, #7974, #2776 ) ;
#10915 = AXIS2_PLACEMENT_3D ( 'NONE', #3584, #4619, #8875 ) ;
#10916 = AXIS2_PLACEMENT_3D ( 'NONE', #963, #2231, #12822 ) ;
#10917 = AXIS2_PLACEMENT_3D ( 'NONE', #13521, #6112, #8425 ) ;
#10918 = ORIENTED_EDGE ( 'NONE', *, *, #2910, .T. ) ;
#10919 = ADVANCED_FACE ( 'NONE', ( #10735 ), #7073, .F. ) ;
#10920 = VERTEX_POINT ( 'NONE', #11080 ) ;
#10921 = DIRECTION ( 'NONE',  ( -0.9496839325805417342, 0.3132098788326399541, 0.000000000000000000 ) ) ;
#10922 = EDGE_LOOP ( 'NONE', ( #8811, #9519, #4461, #10102 ) ) ;
#10923 = ORIENTED_EDGE ( 'NONE', *, *, #263, .T. ) ;
#10924 = VERTEX_POINT ( 'NONE', #6874 ) ;
#10925 = ORIENTED_EDGE ( 'NONE', *, *, #12872, .T. ) ;
#10926 = LINE ( 'NONE', #3308, #4415 ) ;
#10927 = DIRECTION ( 'NONE',  ( 0.000000000000000000, 1.000000000000000000, 0.000000000000000000 ) ) ;
#10928 = ORIENTED_EDGE ( 'NONE', *, *, #6645, .T. ) ;
#10929 = LINE ( 'NONE', #10097, #2065 ) ;
#10930 = CIRCLE ( 'NONE', #12487, 9.999999999999994671 ) ;
#10931 = CARTESIAN_POINT ( 'NONE',  ( -17.19663385324080807, 26.94964292449384402, 56.12280092792923369 ) ) ;
#10932 = CIRCLE ( 'NONE', #3807, 24.92993838181874722 ) ;
#10933 = CARTESIAN_POINT ( 'NONE',  ( -18.05918829504999934, 10.97290950744599947, 63.45000000000000284 ) ) ;
#10934 = AXIS2_PLACEMENT_3D ( 'NONE', #2223, #1213, #3267 ) ;
#10935 = CARTESIAN_POINT ( 'NONE',  ( -19.47340185742309870, 26.91028695795525039, 56.84999999999999432 ) ) ;
#10936 = EDGE_CURVE ( 'NONE', #7051, #9534, #13101, .T. ) ;
#10937 = FACE_OUTER_BOUND ( 'NONE', #10416, .T. ) ;
#10938 = ORIENTED_EDGE ( 'NONE', *, *, #3227, .T. ) ;
#10939 = EDGE_CURVE ( 'NONE', #13640, #821, #4790, .T. ) ;
#10940 = AXIS2_PLACEMENT_3D ( 'NONE', #11258, #627, #11320 ) ;
#10941 = AXIS2_PLACEMENT_3D ( 'NONE', #11833, #12748, #8613 ) ;
#10942 = ORIENTED_EDGE ( 'NONE', *, *, #10046, .F. ) ;
#10943 = ORIENTED_EDGE ( 'NONE', *, *, #11700, .T. ) ;
#10944 = LINE ( 'NONE', #8039, #6780 ) ;
#10945 = ORIENTED_EDGE ( 'NONE', *, *, #2809, .T. ) ;
#10946 = DIRECTION ( 'NONE',  ( -0.000000000000000000, -0.000000000000000000, -1.000000000000000000 ) ) ;
#10947 = LINE ( 'NONE', #12051, #6863 ) ;
#10948 = CARTESIAN_POINT ( 'NONE',  ( -21.59115454767725240, 30.09020406746190446, 55.67294371425958843 ) ) ;
#10949 = CARTESIAN_POINT ( 'NONE',  ( 8.500000000000003553, 2.499999999999999556, 0.000000000000000000 ) ) ;
#10950 = ORIENTED_EDGE ( 'NONE', *, *, #9557, .T. ) ;
#10951 = DIRECTION ( 'NONE',  ( 0.000000000000000000, 0.000000000000000000, -1.000000000000000000 ) ) ;
#10952 = LINE ( 'NONE', #1573, #11582 ) ;
#10953 = DIRECTION ( 'NONE',  ( -1.000000000000000000, 0.000000000000000000, 0.000000000000000000 ) ) ;
#10954 = DIRECTION ( 'NONE',  ( -0.000000000000000000, -0.000000000000000000, -1.000000000000000000 ) ) ;
#10955 = CIRCLE ( 'NONE', #4919, 0.4999999999999991673 ) ;
#10956 = PRODUCT_DEFINITION_SHAPE ( 'NONE', 'NONE',  #13813 ) ;
#10957 = AXIS2_PLACEMENT_3D ( 'NONE', #12368, #3916, #3649 ) ;
#10958 =( NAMED_UNIT ( * ) SI_UNIT ( $, .STERADIAN. ) SOLID_ANGLE_UNIT ( ) );
#10959 = CIRCLE ( 'NONE', #908, 3.000000000000002665 ) ;
#10960 = EDGE_CURVE ( 'NONE', #7761, #2189, #8836, .T. ) ;
#10961 = ORIENTED_EDGE ( 'NONE', *, *, #998, .T. ) ;
#10962 = VERTEX_POINT ( 'NONE', #458 ) ;
#10963 = CIRCLE ( 'NONE', #10077, 2.000000000000001776 ) ;
#10964 =( BOUNDED_CURVE ( )  B_SPLINE_CURVE ( 3, ( #9725, #1412, #10008, #3716 ),
 .UNSPECIFIED., .F., .F. ) 
 B_SPLINE_CURVE_WITH_KNOTS ( ( 4, 4 ),
 ( 0.000000000000000000, 1.000000000000000000 ),
 .UNSPECIFIED. ) 
 CURVE ( )  GEOMETRIC_REPRESENTATION_ITEM ( )  RATIONAL_B_SPLINE_CURVE ( ( 0.9565783017328519655, 0.3188594339109505071, 0.3188594339109505071, 0.9565783017328519655 ) ) 
 REPRESENTATION_ITEM ( '' )  );
#10965 = CARTESIAN_POINT ( 'NONE',  ( -7.499999999999996447, -0.5000000000000017764, -65.00000000000000000 ) ) ;
#10966 = AXIS2_PLACEMENT_3D ( 'NONE', #606, #4874, #11096 ) ;
#10967 = LINE ( 'NONE', #10120, #3798 ) ;
#10968 = AXIS2_PLACEMENT_3D ( 'NONE', #4878, #13463, #1728 ) ;
#10969 = EDGE_LOOP ( 'NONE', ( #1900, #5870, #6499, #1620 ) ) ;
#10970 = EDGE_CURVE ( 'NONE', #6660, #2183, #13303, .T. ) ;
#10971 = ORIENTED_EDGE ( 'NONE', *, *, #599, .F. ) ;
#10972 = CARTESIAN_POINT ( 'NONE',  ( -9.640422211807251784, -16.89844320975769776, 7.000000000000000000 ) ) ;
#10973 = CARTESIAN_POINT ( 'NONE',  ( -18.05918829504999934, 10.97290950744599947, 53.85000000000000142 ) ) ;
#10974 = CARTESIAN_POINT ( 'NONE',  ( -3.759188295049999518, 27.97290950744599769, 64.85000000000000853 ) ) ;
#10975 = DIRECTION ( 'NONE',  ( 0.000000000000000000, 1.000000000000000000, 0.000000000000000000 ) ) ;
#10976 = DIRECTION ( 'NONE',  ( -1.000000000000000000, 0.000000000000000000, 0.000000000000000000 ) ) ;
#10977 = CARTESIAN_POINT ( 'NONE',  ( -25.33503448090910126, 29.19143287883919768, 7.250000000000000000 ) ) ;
#10978 = DIRECTION ( 'NONE',  ( -1.000000000000000000, -0.000000000000000000, -0.000000000000000000 ) ) ;
#10979 = DIRECTION ( 'NONE',  ( -1.000000000000000000, 0.000000000000000000, 0.000000000000000000 ) ) ;
#10980 = DIRECTION ( 'NONE',  ( 0.000000000000000000, 0.000000000000000000, 1.000000000000000000 ) ) ;
#10981 = CIRCLE ( 'NONE', #692, 1.500000000000001332 ) ;
#10982 = CIRCLE ( 'NONE', #4936, 4.250000000000000000 ) ;
#10983 = AXIS2_PLACEMENT_3D ( 'NONE', #5198, #12545, #12676 ) ;
#10984 = DIRECTION ( 'NONE',  ( 1.000000000000000000, 0.000000000000000000, 0.000000000000000000 ) ) ;
#10985 = ADVANCED_FACE ( 'NONE', ( #11144 ), #4729, .T. ) ;
#10986 = ADVANCED_FACE ( 'NONE', ( #1572 ), #3570, .F. ) ;
#10987 = EDGE_LOOP ( 'NONE', ( #9251, #12783 ) ) ;
#10988 = DIRECTION ( 'NONE',  ( -0.9496839325805432885, 0.3132098788326353467, 0.000000000000000000 ) ) ;
#10989 = CARTESIAN_POINT ( 'NONE',  ( 134.6356359024541973, 103.9054980190242361, 22.75000000000000000 ) ) ;
#10990 = EDGE_CURVE ( 'NONE', #10379, #3647, #7851, .T. ) ;
#10991 = CARTESIAN_POINT ( 'NONE',  ( -16.04064420431702942, 4.500000000000000000, -7.307586582922258600 ) ) ;
#10992 = FACE_OUTER_BOUND ( 'NONE', #11719, .T. ) ;
#10993 = DIRECTION ( 'NONE',  ( -1.000000000000000000, 0.000000000000000000, 0.000000000000000000 ) ) ;
#10994 = COLOUR_RGB ( '', 0.66274510, 0.83137255, 0.94901961) ;
#10995 = ORIENTED_EDGE ( 'NONE', *, *, #4413, .T. ) ;
#10996 = DIRECTION ( 'NONE',  ( -0.7498604124941127269, -0.6615960714621567096, 0.000000000000000000 ) ) ;
#10997 = VERTEX_POINT ( 'NONE', #326 ) ;
#10998 = EDGE_CURVE ( 'NONE', #8025, #7886, #8379, .T. ) ;
#10999 = ORIENTED_EDGE ( 'NONE', *, *, #11880, .F. ) ;
#11000 = ORIENTED_EDGE ( 'NONE', *, *, #12183, .F. ) ;
#11001 = CARTESIAN_POINT ( 'NONE',  ( -19.55918829504999934, 27.90660372932210009, 57.35000000000000142 ) ) ;
#11002 = DIRECTION ( 'NONE',  ( 0.7498604124941127269, 0.6615960714621567096, 0.000000000000000000 ) ) ;
#11003 = VERTEX_POINT ( 'NONE', #7917 ) ;
#11004 = DIRECTION ( 'NONE',  ( -0.000000000000000000, -0.000000000000000000, 1.000000000000000000 ) ) ;
#11005 = AXIS2_PLACEMENT_3D ( 'NONE', #4096, #2078, #8344 ) ;
#11006 = CARTESIAN_POINT ( 'NONE',  ( -30.30918829504999934, 27.97290950744599769, 7.250000000000000000 ) ) ;
#11007 = DIRECTION ( 'NONE',  ( -0.000000000000000000, -0.000000000000000000, 1.000000000000000000 ) ) ;
#11008 = EDGE_CURVE ( 'NONE', #7689, #1569, #13139, .T. ) ;
#11009 = CARTESIAN_POINT ( 'NONE',  ( -40.05918829505000645, 35.97290950744599769, 0.000000000000000000 ) ) ;
#11010 =( REPRESENTATION_RELATIONSHIP ('NONE','NONE', #11848, #12309 ) REPRESENTATION_RELATIONSHIP_WITH_TRANSFORMATION ( #5397 )SHAPE_REPRESENTATION_RELATIONSHIP( ) );
#11011 = AXIS2_PLACEMENT_3D ( 'NONE', #6931, #7061, #10229 ) ;
#11012 = ORIENTED_EDGE ( 'NONE', *, *, #161, .F. ) ;
#11013 = EDGE_CURVE ( 'NONE', #3980, #4904, #10667, .T. ) ;
#11014 = VERTEX_POINT ( 'NONE', #7780 ) ;
#11015 = DIRECTION ( 'NONE',  ( 0.000000000000000000, 0.000000000000000000, 1.000000000000000000 ) ) ;
#11016 = FACE_OUTER_BOUND ( 'NONE', #2312, .T. ) ;
#11017 = ADVANCED_FACE ( 'NONE', ( #12054 ), #11020, .T. ) ;
#11018 = CARTESIAN_POINT ( 'NONE',  ( -21.62262619219993454, 30.08533272846090512, 55.76115953722869989 ) ) ;
#11019 = DIRECTION ( 'NONE',  ( 0.000000000000000000, 0.000000000000000000, -1.000000000000000000 ) ) ;
#11020 = CYLINDRICAL_SURFACE ( 'NONE', #12674, 6.449999999999997513 ) ;
#11021 = LINE ( 'NONE', #5753, #13798 ) ;
#11022 = FACE_OUTER_BOUND ( 'NONE', #8679, .T. ) ;
#11023 = EDGE_CURVE ( 'NONE', #12924, #2075, #5680, .T. ) ;
#11024 = AXIS2_PLACEMENT_3D ( 'NONE', #611, #10389, #813 ) ;
#11025 = CARTESIAN_POINT ( 'NONE',  ( 0.000000000000000000, 0.000000000000000000, 0.000000000000000000 ) ) ;
#11026 = EDGE_LOOP ( 'NONE', ( #2068, #1850, #11244, #8615 ) ) ;
#11027 = ORIENTED_EDGE ( 'NONE', *, *, #2178, .T. ) ;
#11028 = CARTESIAN_POINT ( 'NONE',  ( -1.059188295049996231, 27.97290950744599769, 83.57661607529820458 ) ) ;
#11029 = ORIENTED_EDGE ( 'NONE', *, *, #8598, .T. ) ;
#11030 = CARTESIAN_POINT ( 'NONE',  ( 116.7775623211734342, 85.03908161011133870, 19.25000000000000000 ) ) ;
#11031 = DIRECTION ( 'NONE',  ( 0.000000000000000000, 0.000000000000000000, 1.000000000000000000 ) ) ;
#11032 = DIRECTION ( 'NONE',  ( 0.000000000000000000, 0.000000000000000000, 1.000000000000000000 ) ) ;
#11033 = DIRECTION ( 'NONE',  ( 0.000000000000000000, -1.000000000000000000, 0.000000000000000000 ) ) ;
#11034 = CARTESIAN_POINT ( 'NONE',  ( -40.33164489498318517, 10.97290950744599947, 83.57661607529820458 ) ) ;
#11035 = FACE_OUTER_BOUND ( 'NONE', #8903, .T. ) ;
#11036 = LINE ( 'NONE', #10059, #3110 ) ;
#11037 = DIRECTION ( 'NONE',  ( 0.000000000000000000, 0.000000000000000000, -1.000000000000000000 ) ) ;
#11038 = EDGE_CURVE ( 'NONE', #8205, #3796, #2883, .T. ) ;
#11039 = DIRECTION ( 'NONE',  ( 0.4528443260392610026, 0.8915896008669278450, 0.000000000000000000 ) ) ;
#11040 = LINE ( 'NONE', #5911, #13118 ) ;
#11041 = ORIENTED_EDGE ( 'NONE', *, *, #972, .F. ) ;
#11042 = EDGE_LOOP ( 'NONE', ( #2772, #12859, #9846, #3832 ) ) ;
#11043 = DIRECTION ( 'NONE',  ( 0.000000000000000000, 1.000000000000000000, 0.000000000000000000 ) ) ;
#11044 = EDGE_LOOP ( 'NONE', ( #3150, #10089, #4438, #567 ) ) ;
#11045 = VERTEX_POINT ( 'NONE', #8997 ) ;
#11046 = CARTESIAN_POINT ( 'NONE',  ( -3.759188295049999518, -6.027090492554000534, 58.85000000000000142 ) ) ;
#11047 = SURFACE_SIDE_STYLE ('',( #2547 ) ) ;
#11048 = CARTESIAN_POINT ( 'NONE',  ( -21.69796668809184936, 15.09714177616359798, 30.59999999999999787 ) ) ;
#11049 = AXIS2_PLACEMENT_3D ( 'NONE', #4356, #219, #9804 ) ;
#11050 = CARTESIAN_POINT ( 'NONE',  ( -1.461186629049982422, 2.673908674445990119, 63.13003331700004850 ) ) ;
#11051 = FACE_BOUND ( 'NONE', #7579, .T. ) ;
#11052 = EDGE_CURVE ( 'NONE', #6829, #7790, #12144, .T. ) ;
#11053 = EDGE_CURVE ( 'NONE', #13024, #13765, #9098, .T. ) ;
#11054 = ORIENTED_EDGE ( 'NONE', *, *, #9984, .T. ) ;
#11055 = EDGE_CURVE ( 'NONE', #1279, #2935, #4650, .T. ) ;
#11056 = AXIS2_PLACEMENT_3D ( 'NONE', #2674, #9067, #1397 ) ;
#11057 = DIRECTION ( 'NONE',  ( -1.000000000000000000, 0.000000000000000000, 0.000000000000000000 ) ) ;
#11058 = ORIENTED_EDGE ( 'NONE', *, *, #12098, .F. ) ;
#11059 = ORIENTED_EDGE ( 'NONE', *, *, #9988, .T. ) ;
#11060 = PRODUCT_DEFINITION_SHAPE ( 'NONE', 'NONE',  #13807 ) ;
#11061 = ORIENTED_EDGE ( 'NONE', *, *, #13497, .T. ) ;
#11062 = CARTESIAN_POINT ( 'NONE',  ( -18.05918829504999934, 10.97290950744599947, 68.84999999999999432 ) ) ;
#11063 = CARTESIAN_POINT ( 'NONE',  ( -18.05918829504999934, 28.64232754551664684, 57.35000000000000142 ) ) ;
#11064 = ORIENTED_EDGE ( 'NONE', *, *, #3455, .F. ) ;
#11065 = CYLINDRICAL_SURFACE ( 'NONE', #9869, 1.999999999999993117 ) ;
#11066 = CARTESIAN_POINT ( 'NONE',  ( -25.86749127492459976, 30.80589556422609832, 17.25000000000000000 ) ) ;
#11067 = DIRECTION ( 'NONE',  ( 1.000000000000000000, 0.000000000000000000, 0.000000000000000000 ) ) ;
#11068 = AXIS2_PLACEMENT_3D ( 'NONE', #1716, #9267, #6461 ) ;
#11069 = CYLINDRICAL_SURFACE ( 'NONE', #9384, 3.000000000000002665 ) ;
#11070 = EDGE_LOOP ( 'NONE', ( #13146, #12549 ) ) ;
#11071 = ADVANCED_FACE ( 'NONE', ( #7933 ), #4673, .T. ) ;
#11072 = ORIENTED_EDGE ( 'NONE', *, *, #5417, .F. ) ;
#11073 = ADVANCED_FACE ( 'NONE', ( #539 ), #338, .F. ) ;
#11074 = PRODUCT_DEFINITION ( 'UNKNOWN', '', #10470, #13527 ) ;
#11075 = VECTOR ( 'NONE', #6666, 1000.000000000000000 ) ;
#11076 = CARTESIAN_POINT ( 'NONE',  ( -8.814269998155332075, 15.06602133594271820, 0.000000000000000000 ) ) ;
#11077 = CYLINDRICAL_SURFACE ( 'NONE', #831, 3.000000000000000000 ) ;
#11078 = CARTESIAN_POINT ( 'NONE',  ( -20.85091026108096557, 30.19191053445972628, 60.32389291502525452 ) ) ;
#11079 = CYLINDRICAL_SURFACE ( 'NONE', #12097, 4.750000000000000888 ) ;
#11080 = CARTESIAN_POINT ( 'NONE',  ( -25.86749127492460332, 30.80589556422609832, 17.25000000000000000 ) ) ;
#11081 = CARTESIAN_POINT ( 'NONE',  ( 3.500000000000001776, 2.499999999999999556, -65.00000000000000000 ) ) ;
#11082 = DIRECTION ( 'NONE',  ( -1.000000000000000000, 0.000000000000000000, 0.000000000000000000 ) ) ;
#11083 = CYLINDRICAL_SURFACE ( 'NONE', #5123, 24.03999999999999915 ) ;
#11084 =( NAMED_UNIT ( * ) SI_UNIT ( $, .STERADIAN. ) SOLID_ANGLE_UNIT ( ) );
#11085 = ORIENTED_EDGE ( 'NONE', *, *, #1854, .F. ) ;
#11086 = ADVANCED_FACE ( 'NONE', ( #5635 ), #5768, .T. ) ;
#11087 = AXIS2_PLACEMENT_3D ( 'NONE', #8235, #3915, #2878 ) ;
#11088 = ORIENTED_EDGE ( 'NONE', *, *, #6323, .F. ) ;
#11089 = VERTEX_POINT ( 'NONE', #6821 ) ;
#11090 = EDGE_CURVE ( 'NONE', #1604, #8398, #168, .T. ) ;
#11091 = FACE_OUTER_BOUND ( 'NONE', #13037, .T. ) ;
#11092 = DIRECTION ( 'NONE',  ( 0.000000000000000000, 0.000000000000000000, 1.000000000000000000 ) ) ;
#11093 = CARTESIAN_POINT ( 'NONE',  ( -0.04028432657539327000, 4.500000000000000000, 20.54539866546728533 ) ) ;
#11094 = PRESENTATION_STYLE_ASSIGNMENT (( #6957 ) ) ;
#11095 = PLANE ( 'NONE',  #6420 ) ;
#11096 = DIRECTION ( 'NONE',  ( -1.000000000000000000, 0.000000000000000000, 0.000000000000000000 ) ) ;
#11097 = FACE_OUTER_BOUND ( 'NONE', #1425, .T. ) ;
#11098 = DIRECTION ( 'NONE',  ( -0.000000000000000000, -1.000000000000000000, -0.000000000000000000 ) ) ;
#11099 = DIRECTION ( 'NONE',  ( 0.000000000000000000, 0.000000000000000000, -1.000000000000000000 ) ) ;
#11100 = CARTESIAN_POINT ( 'NONE',  ( 2.262399129208274129, 22.44393519180576746, 17.25000000000000000 ) ) ;
#11101 = CYLINDRICAL_SURFACE ( 'NONE', #6546, 6.449999999999997513 ) ;
#11102 = DIRECTION ( 'NONE',  ( 0.000000000000000000, 0.000000000000000000, 1.000000000000000000 ) ) ;
#11103 = ADVANCED_FACE ( 'NONE', ( #1307 ), #3690, .F. ) ;
#11104 = AXIS2_PLACEMENT_3D ( 'NONE', #5968, #10453, #2863 ) ;
#11105 = EDGE_CURVE ( 'NONE', #13747, #7886, #7653, .T. ) ;
#11106 = ORIENTED_EDGE ( 'NONE', *, *, #10536, .T. ) ;
#11107 = FACE_OUTER_BOUND ( 'NONE', #4093, .T. ) ;
#11108 = ORIENTED_EDGE ( 'NONE', *, *, #2393, .T. ) ;
#11109 = CARTESIAN_POINT ( 'NONE',  ( -40.33164489498319938, 10.97290950744599947, 17.25000000000000000 ) ) ;
#11110 = FACE_OUTER_BOUND ( 'NONE', #4219, .T. ) ;
#11111 = CARTESIAN_POINT ( 'NONE',  ( 44.63563590245420443, 94.90549801902425031, 23.00000000000000000 ) ) ;
#11112 = AXIS2_PLACEMENT_3D ( 'NONE', #11693, #13706, #3835 ) ;
#11113 = CARTESIAN_POINT ( 'NONE',  ( -20.57325336660620252, 13.82237907492362083, 27.09999999999999787 ) ) ;
#11114 = CIRCLE ( 'NONE', #1734, 8.395833332999997012 ) ;
#11115 = DIRECTION ( 'NONE',  ( 0.7071067811865525687, 0.7071067811865425767, -0.000000000000000000 ) ) ;
#11116 = CARTESIAN_POINT ( 'NONE',  ( -7.640422211807256225, -16.89844320975769776, 7.000000000000000000 ) ) ;
#11117 = CONICAL_SURFACE ( 'NONE', #5088, 5.000000000000000888, 0.7853981633974497223 ) ;
#11118 = ORIENTED_EDGE ( 'NONE', *, *, #6115, .T. ) ;
#11119 = CIRCLE ( 'NONE', #12462, 0.7499999999999966693 ) ;
#11120 = AXIS2_PLACEMENT_3D ( 'NONE', #885, #1943, #8219 ) ;
#11121 = ORIENTED_EDGE ( 'NONE', *, *, #130, .T. ) ;
#11122 = VECTOR ( 'NONE', #12602, 1000.000000000000000 ) ;
#11123 = ORIENTED_EDGE ( 'NONE', *, *, #12942, .F. ) ;
#11124 = CARTESIAN_POINT ( 'NONE',  ( -16.40830210679616741, 30.30175501171254382, 61.28060770126166545 ) ) ;
#11125 = ORIENTED_EDGE ( 'NONE', *, *, #2906, .T. ) ;
#11126 = EDGE_LOOP ( 'NONE', ( #6646, #5472, #9803, #11546 ) ) ;
#11127 = ORIENTED_EDGE ( 'NONE', *, *, #7268, .T. ) ;
#11128 = CARTESIAN_POINT ( 'NONE',  ( -18.05918829505001355, 18.58149382944599992, 61.98378871700002435 ) ) ;
#11129 = ADVANCED_FACE ( 'NONE', ( #1590 ), #1287, .T. ) ;
#11130 = CARTESIAN_POINT ( 'NONE',  ( -43.05918829505001355, -11.02709049255400053, 10.00000000000000000 ) ) ;
#11131 = ORIENTED_EDGE ( 'NONE', *, *, #1969, .T. ) ;
#11132 = CARTESIAN_POINT ( 'NONE',  ( -14.08961186627706041, 6.473747032481329988, 64.85000000000000853 ) ) ;
#11133 = CARTESIAN_POINT ( 'NONE',  ( -18.05918829504999934, 10.97290950744599947, 64.85000000000000853 ) ) ;
#11134 = AXIS2_PLACEMENT_3D ( 'NONE', #2611, #9438, #11519 ) ;
#11135 = DIRECTION ( 'NONE',  ( 0.000000000000000000, 0.000000000000000000, -1.000000000000000000 ) ) ;
#11136 = TOROIDAL_SURFACE ( 'NONE', #864, 20.00000000000000000, 1.500000000000000000 ) ;
#11137 = LINE ( 'NONE', #1563, #8707 ) ;
#11138 = AXIS2_PLACEMENT_3D ( 'NONE', #8281, #12609, #7078 ) ;
#11139 = CYLINDRICAL_SURFACE ( 'NONE', #12184, 0.9499999999999995115 ) ;
#11140 = EDGE_CURVE ( 'NONE', #10620, #11879, #6890, .T. ) ;
#11141 = FACE_OUTER_BOUND ( 'NONE', #3519, .T. ) ;
#11142 = CARTESIAN_POINT ( 'NONE',  ( -21.72501355060861528, 30.06926057631531535, 58.60720357358517418 ) ) ;
#11143 = CARTESIAN_POINT ( 'NONE',  ( -12.62505638257885998, 21.67198471784914915, 61.85000000000000142 ) ) ;
#11144 = FACE_OUTER_BOUND ( 'NONE', #12768, .T. ) ;
#11145 = DIRECTION ( 'NONE',  ( 0.000000000000000000, 0.000000000000000000, -1.000000000000000000 ) ) ;
#11146 = CARTESIAN_POINT ( 'NONE',  ( 185.2712718049083946, 0.000000000000000000, 23.00000000000000000 ) ) ;
#11147 = FACE_OUTER_BOUND ( 'NONE', #1135, .T. ) ;
#11148 = DIRECTION ( 'NONE',  ( 1.000000000000000000, 0.000000000000000000, 0.000000000000000000 ) ) ;
#11149 = AXIS2_PLACEMENT_3D ( 'NONE', #12504, #10210, #5024 ) ;
#11150 = AXIS2_PLACEMENT_3D ( 'NONE', #389, #8780, #2377 ) ;
#11151 = DIRECTION ( 'NONE',  ( 0.4678190685372678459, -0.5302313826179257950, 0.7071067811865516806 ) ) ;
#11152 = VERTEX_POINT ( 'NONE', #2389 ) ;
#11153 = CYLINDRICAL_SURFACE ( 'NONE', #5799, 16.95000000000000284 ) ;
#11154 = ADVANCED_FACE ( 'NONE', ( #2591 ), #11095, .F. ) ;
#11155 = CARTESIAN_POINT ( 'NONE',  ( 16.04064420431708982, 4.500000000000000000, 11.30758658292213248 ) ) ;
#11156 = CARTESIAN_POINT ( 'NONE',  ( 140.6356359024541973, 113.0390816101113387, 20.00000000000000000 ) ) ;
#11157 = DIRECTION ( 'NONE',  ( 0.000000000000000000, 1.000000000000000000, 0.000000000000000000 ) ) ;
#11158 = AXIS2_PLACEMENT_3D ( 'NONE', #11028, #8005, #13381 ) ;
#11159 = CIRCLE ( 'NONE', #6915, 1.999999999999994893 ) ;
#11160 = DIRECTION ( 'NONE',  ( 0.6615960714621564875, -0.7498604124941129490, 0.000000000000000000 ) ) ;
#11161 = CARTESIAN_POINT ( 'NONE',  ( 68.49370948373500312, 85.03908161011133870, 19.25000000000000000 ) ) ;
#11162 = CARTESIAN_POINT ( 'NONE',  ( -7.241070169793063727, -7.867426463707971607, 5.250000000000000000 ) ) ;
#11163 = CARTESIAN_POINT ( 'NONE',  ( -20.04397650943645459, 13.22249074492834175, 27.09999999999999787 ) ) ;
#11164 = ADVANCED_FACE ( 'NONE', ( #4537 ), #5563, .T. ) ;
#11165 = CARTESIAN_POINT ( 'NONE',  ( -18.05918829504999934, 10.97290950744599947, 57.35000000000000142 ) ) ;
#11166 = DIRECTION ( 'NONE',  ( 1.000000000000000000, 2.775557561562892929E-15, 0.000000000000000000 ) ) ;
#11167 = ADVANCED_FACE ( 'NONE', ( #1448 ), #7791, .F. ) ;
#11168 = VECTOR ( 'NONE', #8849, 1000.000000000000000 ) ;
#11169 = AXIS2_PLACEMENT_3D ( 'NONE', #5187, #11685, #1050 ) ;
#11170 = VECTOR ( 'NONE', #2837, 1000.000000000000000 ) ;
#11171 = VERTEX_POINT ( 'NONE', #5697 ) ;
#11172 = EDGE_LOOP ( 'NONE', ( #12171, #2557, #8751, #9396 ) ) ;
#11173 = CARTESIAN_POINT ( 'NONE',  ( -1.059188295049996231, -6.027090492554000534, 64.85000000000000853 ) ) ;
#11174 = ORIENTED_EDGE ( 'NONE', *, *, #12420, .F. ) ;
#11176 = ORIENTED_EDGE ( 'NONE', *, *, #468, .F. ) ;
#11175 = ADVANCED_FACE ( 'NONE', ( #402 ), #10639, .F. ) ;
#11177 = DIRECTION ( 'NONE',  ( 1.000000000000000000, 0.000000000000000000, 0.000000000000000000 ) ) ;
#11178 = FACE_BOUND ( 'NONE', #10621, .T. ) ;
#11179 =( NAMED_UNIT ( * ) SI_UNIT ( $, .STERADIAN. ) SOLID_ANGLE_UNIT ( ) );
#11180 = FACE_OUTER_BOUND ( 'NONE', #10602, .T. ) ;
#11181 = AXIS2_PLACEMENT_3D ( 'NONE', #13721, #4171, #12686 ) ;
#11182 = VECTOR ( 'NONE', #4943, 1000.000000000000000 ) ;
#11183 = DIRECTION ( 'NONE',  ( 0.7091883091770476710, -0.7050191076322684935, 0.000000000000000000 ) ) ;
#11184 = VECTOR ( 'NONE', #12695, 1000.000000000000000 ) ;
#11185 = CARTESIAN_POINT ( 'NONE',  ( -8.499999999999998224, 2.000000000000000000, 0.000000000000000000 ) ) ;
#11186 = EDGE_CURVE ( 'NONE', #13219, #11645, #2652, .T. ) ;
#11187 = FACE_OUTER_BOUND ( 'NONE', #7315, .T. ) ;
#11188 = ORIENTED_EDGE ( 'NONE', *, *, #468, .T. ) ;
#11189 = EDGE_LOOP ( 'NONE', ( #7317, #4594, #6373, #7901 ) ) ;
#11190 =( GEOMETRIC_REPRESENTATION_CONTEXT ( 3 ) GLOBAL_UNCERTAINTY_ASSIGNED_CONTEXT ( ( #1527 ) ) GLOBAL_UNIT_ASSIGNED_CONTEXT ( ( #2265, #10768, #12788 ) ) REPRESENTATION_CONTEXT ( 'NONE', 'WORKASPACE' ) );
#11191 = ORIENTED_EDGE ( 'NONE', *, *, #10846, .F. ) ;
#11192 = CARTESIAN_POINT ( 'NONE',  ( -16.13055293506123888, 30.28009008632742649, 61.11049587954376960 ) ) ;
#11193 = CIRCLE ( 'NONE', #5169, 18.00000000000000000 ) ;
#11194 = VERTEX_POINT ( 'NONE', #11547 ) ;
#11195 = ORIENTED_EDGE ( 'NONE', *, *, #10824, .T. ) ;
#11196 = ORIENTED_EDGE ( 'NONE', *, *, #9908, .T. ) ;
#11197 = CARTESIAN_POINT ( 'NONE',  ( -5.631644894983189431, 10.97290950744599947, 83.57661607529820458 ) ) ;
#11198 = ORIENTED_EDGE ( 'NONE', *, *, #5254, .T. ) ;
#11199 = B_SPLINE_CURVE_WITH_KNOTS ( 'NONE', 3,
 ( #273, #13044, #8570, #11664, #6347, #3223, #12774, #10608, #5286, #9559, #13796, #4266, #8508 ),
 .UNSPECIFIED., .F., .F.,
 ( 4, 1, 1, 1, 1, 1, 2, 2, 4 ),
 ( 0.000000000000000000, 0.2499999999999915623, 0.3749999999999858447, 0.4374999999999851785, 0.4687499999999875100, 0.4843749999999908407, 0.4921874999999919509, 0.4999999999999930056, 1.000000000000000000 ),
 .UNSPECIFIED. ) ;
#11200 = DIRECTION ( 'NONE',  ( 0.000000000000000000, 0.000000000000000000, 1.000000000000000000 ) ) ;
#11201 = ORIENTED_EDGE ( 'NONE', *, *, #12117, .F. ) ;
#11202 = CARTESIAN_POINT ( 'NONE',  ( -33.27635693905001801, 3.364325185445997679, 61.98378871700000303 ) ) ;
#11203 = CYLINDRICAL_SURFACE ( 'NONE', #10022, 6.449999999999997513 ) ;
#11204 = ORIENTED_EDGE ( 'NONE', *, *, #2198, .F. ) ;
#11205 = CARTESIAN_POINT ( 'NONE',  ( -16.04064420431702942, 0.000000000000000000, -9.307586582922249718 ) ) ;
#11206 = CARTESIAN_POINT ( 'NONE',  ( -32.35918829505000360, 27.97290950744599769, 7.250000000000000000 ) ) ;
#11207 = DIRECTION ( 'NONE',  ( 0.000000000000000000, 0.000000000000000000, -1.000000000000000000 ) ) ;
#11208 = ADVANCED_FACE ( 'NONE', ( #2865 ), #2734, .F. ) ;
#11209 = DIRECTION ( 'NONE',  ( -1.000000000000000000, 0.000000000000000000, 0.000000000000000000 ) ) ;
#11210 = AXIS2_PLACEMENT_3D ( 'NONE', #4392, #5225, #8721 ) ;
#11211 = EDGE_CURVE ( 'NONE', #5173, #12738, #412, .T. ) ;
#11212 = ORIENTED_EDGE ( 'NONE', *, *, #7912, .F. ) ;
#11213 = ORIENTED_EDGE ( 'NONE', *, *, #2502, .F. ) ;
#11214 = EDGE_LOOP ( 'NONE', ( #11800, #12120, #8257, #13074 ) ) ;
#11215 = VECTOR ( 'NONE', #384, 1000.000000000000000 ) ;
#11216 = DIRECTION ( 'NONE',  ( 0.000000000000000000, 0.000000000000000000, 1.000000000000000000 ) ) ;
#11217 =( NAMED_UNIT ( * ) PLANE_ANGLE_UNIT ( ) SI_UNIT ( $, .RADIAN. ) );
#11218 = CARTESIAN_POINT ( 'NONE',  ( -21.80266211316538616, 30.05678106875573263, 58.27625053142192968 ) ) ;
#11219 = DIRECTION ( 'NONE',  ( 1.000000000000000000, 0.000000000000000000, 0.000000000000000000 ) ) ;
#11220 = DIRECTION ( 'NONE',  ( -0.7071067811865505703, 8.659560562354931626E-17, 0.7071067811865444641 ) ) ;
#11221 = CARTESIAN_POINT ( 'NONE',  ( -18.05918829504999934, 10.97290950744599947, 61.86500000000000199 ) ) ;
#11222 = FACE_OUTER_BOUND ( 'NONE', #12426, .T. ) ;
#11223 = ORIENTED_EDGE ( 'NONE', *, *, #12294, .T. ) ;
#11224 = CIRCLE ( 'NONE', #12113, 2.700000000000001066 ) ;
#11225 = EDGE_CURVE ( 'NONE', #10360, #1687, #393, .T. ) ;
#11226 = EDGE_CURVE ( 'NONE', #8282, #12380, #5902, .T. ) ;
#11227 = LINE ( 'NONE', #7084, #13731 ) ;
#11228 = CARTESIAN_POINT ( 'NONE',  ( -18.05918829504999934, 10.00028003023991907, 62.14999999999999858 ) ) ;
#11229 = ORIENTED_EDGE ( 'NONE', *, *, #2264, .F. ) ;
#11230 = DIRECTION ( 'NONE',  ( -0.9496839325805421783, 0.3132098788326385663, 0.000000000000000000 ) ) ;
#11231 = CYLINDRICAL_SURFACE ( 'NONE', #3733, 1.999999999999991340 ) ;
#11232 = DIRECTION ( 'NONE',  ( 1.000000000000000000, 0.000000000000000000, 0.000000000000000000 ) ) ;
#11233 = CIRCLE ( 'NONE', #12354, 5.000000000000000888 ) ;
#11234 = DIRECTION ( 'NONE',  ( 0.000000000000000000, 0.000000000000000000, -1.000000000000000000 ) ) ;
#11235 = DIRECTION ( 'NONE',  ( 1.000000000000000000, 0.000000000000000000, 0.000000000000000000 ) ) ;
#11236 = CARTESIAN_POINT ( 'NONE',  ( -16.45469220996245596, -1.832421873814834123, 0.000000000000000000 ) ) ;
#11237 = DIRECTION ( 'NONE',  ( 0.3202092937642119774, 0.6304490528084099044, -0.7071067811865499042 ) ) ;
#11238 = FACE_OUTER_BOUND ( 'NONE', #13086, .T. ) ;
#11239 = CARTESIAN_POINT ( 'NONE',  ( -35.05918829505000645, 27.97290950744599769, 0.000000000000000000 ) ) ;
#11240 = DIRECTION ( 'NONE',  ( 0.000000000000000000, 0.000000000000000000, 1.000000000000000000 ) ) ;
#11241 = EDGE_CURVE ( 'NONE', #11264, #11802, #10188, .T. ) ;
#11242 = VECTOR ( 'NONE', #6149, 1000.000000000000000 ) ;
#11243 = EDGE_CURVE ( 'NONE', #10451, #322, #2196, .T. ) ;
#11244 = ORIENTED_EDGE ( 'NONE', *, *, #8576, .T. ) ;
#11245 = ORIENTED_EDGE ( 'NONE', *, *, #5603, .F. ) ;
#11246 = ORIENTED_EDGE ( 'NONE', *, *, #10599, .T. ) ;
#11247 = DIRECTION ( 'NONE',  ( 0.000000000000000000, 0.000000000000000000, 1.000000000000000000 ) ) ;
#11248 = EDGE_LOOP ( 'NONE', ( #12187, #8755, #8328, #8921 ) ) ;
#11249 = ORIENTED_EDGE ( 'NONE', *, *, #559, .F. ) ;
#11250 = ORIENTED_EDGE ( 'NONE', *, *, #11570, .F. ) ;
#11251 = CARTESIAN_POINT ( 'NONE',  ( 134.8856359024541973, 104.1554980190242361, 23.00000000000000000 ) ) ;
#11252 = EDGE_CURVE ( 'NONE', #506, #5782, #6375, .T. ) ;
#11253 = DIRECTION ( 'NONE',  ( 1.000000000000000000, 0.000000000000000000, 0.000000000000000000 ) ) ;
#11254 = EDGE_CURVE ( 'NONE', #2443, #2279, #3191, .T. ) ;
#11255 = SURFACE_STYLE_USAGE ( .BOTH. , #825 ) ;
#11256 = CYLINDRICAL_SURFACE ( 'NONE', #3119, 24.04163056034261459 ) ;
#11257 = DIRECTION ( 'NONE',  ( -1.000000000000000000, 0.000000000000000000, 0.000000000000000000 ) ) ;
#11258 = CARTESIAN_POINT ( 'NONE',  ( -7.499999999999996447, -1.762812401309176307E-15, 0.000000000000000000 ) ) ;
#11259 = DIRECTION ( 'NONE',  ( -1.000000000000000000, 0.000000000000000000, 0.000000000000000000 ) ) ;
#11260 = ADVANCED_FACE ( 'NONE', ( #7267 ), #11341, .T. ) ;
#11261 = ORIENTED_EDGE ( 'NONE', *, *, #11562, .F. ) ;
#11262 = ORIENTED_EDGE ( 'NONE', *, *, #7329, .T. ) ;
#11263 = CARTESIAN_POINT ( 'NONE',  ( -17.79480846713035902, 30.35913048975401551, 61.70128263341860020 ) ) ;
#11264 = VERTEX_POINT ( 'NONE', #5192 ) ;
#11265 = EDGE_CURVE ( 'NONE', #8057, #12302, #6236, .T. ) ;
#11266 = CARTESIAN_POINT ( 'NONE',  ( 44.63563590245420443, 89.90549801902423610, 22.75000000000000000 ) ) ;
#11267 = DIRECTION ( 'NONE',  ( 0.000000000000000000, 0.000000000000000000, -1.000000000000000000 ) ) ;
#11268 = DIRECTION ( 'NONE',  ( 0.9496839325805432885, -0.3132098788326352912, 0.000000000000000000 ) ) ;
#11269 = ORIENTED_EDGE ( 'NONE', *, *, #9877, .T. ) ;
#11270 = CARTESIAN_POINT ( 'NONE',  ( -10.47404583389237942, 25.90703532196704728, 60.65000000000000568 ) ) ;
#11271 = CYLINDRICAL_SURFACE ( 'NONE', #4321, 18.50000000000000000 ) ;
#11272 = CARTESIAN_POINT ( 'NONE',  ( -35.05918829505000645, 27.97290950744599769, 68.85549045786049760 ) ) ;
#11273 = DIRECTION ( 'NONE',  ( -0.000000000000000000, 1.000000000000000000, -0.000000000000000000 ) ) ;
#11274 = EDGE_CURVE ( 'NONE', #803, #12773, #4204, .T. ) ;
#11275 = ORIENTED_EDGE ( 'NONE', *, *, #7150, .F. ) ;
#11276 = ORIENTED_EDGE ( 'NONE', *, *, #3553, .F. ) ;
#11277 = ORIENTED_EDGE ( 'NONE', *, *, #13036, .T. ) ;
#11278 = EDGE_LOOP ( 'NONE', ( #1603, #9727, #8636, #8588 ) ) ;
#11279 = ADVANCED_FACE ( 'NONE', ( #9133 ), #10511, .F. ) ;
#11280 = EDGE_LOOP ( 'NONE', ( #183, #269 ) ) ;
#11281 = CARTESIAN_POINT ( 'NONE',  ( 111.0903281124166710, 100.8715034839261762, 10.00000000000000000 ) ) ;
#11282 = CONICAL_SURFACE ( 'NONE', #6803, 4.546599999999997976, 1.029744258676653645 ) ;
#11283 = CARTESIAN_POINT ( 'NONE',  ( -20.51961422855616490, 30.22970645148964763, 60.68279484739409924 ) ) ;
#11284 = CARTESIAN_POINT ( 'NONE',  ( 8.000000000000000000, -1.762812401309176307E-15, -65.00000000000000000 ) ) ;
#11285 = CARTESIAN_POINT ( 'NONE',  ( -35.05918829505000645, 27.97290950744599769, 64.85000000000000853 ) ) ;
#11286 = DIRECTION ( 'NONE',  ( 0.000000000000000000, 0.000000000000000000, -1.000000000000000000 ) ) ;
#11287 = CARTESIAN_POINT ( 'NONE',  ( 0.000000000000000000, 0.000000000000000000, 7.000000000000000000 ) ) ;
#11288 = APPLICATION_PROTOCOL_DEFINITION ( 'draft international standard', 'automotive_design', 1998, #4316 ) ;
#11289 = VECTOR ( 'NONE', #8287, 1000.000000000000000 ) ;
#11290 = VERTEX_POINT ( 'NONE', #1001 ) ;
#11291 = CARTESIAN_POINT ( 'NONE',  ( -24.10918829505000005, 10.97290950744599947, 0.000000000000000000 ) ) ;
#11292 = ORIENTED_EDGE ( 'NONE', *, *, #6474, .F. ) ;
#11293 = ORIENTED_EDGE ( 'NONE', *, *, #12890, .F. ) ;
#11294 = DIRECTION ( 'NONE',  ( 0.000000000000000000, 0.000000000000000000, 1.000000000000000000 ) ) ;
#11295 = DIRECTION ( 'NONE',  ( 0.000000000000000000, 0.000000000000000000, -1.000000000000000000 ) ) ;
#11296 = DIRECTION ( 'NONE',  ( 0.000000000000000000, -0.000000000000000000, -1.000000000000000000 ) ) ;
#11297 = DIRECTION ( 'NONE',  ( 0.000000000000000000, -0.000000000000000000, 1.000000000000000000 ) ) ;
#11298 = EDGE_LOOP ( 'NONE', ( #10604, #12570, #11041, #3882 ) ) ;
#11299 = DIRECTION ( 'NONE',  ( 0.000000000000000000, 0.000000000000000000, -1.000000000000000000 ) ) ;
#11300 = DIRECTION ( 'NONE',  ( 0.000000000000000000, 0.000000000000000000, 1.000000000000000000 ) ) ;
#11301 = FACE_OUTER_BOUND ( 'NONE', #301, .T. ) ;
#11302 = ADVANCED_FACE ( 'NONE', ( #8083 ), #7021, .F. ) ;
#11303 = CARTESIAN_POINT ( 'NONE',  ( 1.629816981350590055, -4.941769416738769571, 17.25000000000000000 ) ) ;
#11304 = VECTOR ( 'NONE', #1360, 1000.000000000000000 ) ;
#11305 = CARTESIAN_POINT ( 'NONE',  ( -4.599650328638321461, 0.000000000000000000, -9.878124499050780827 ) ) ;
#11306 = DIRECTION ( 'NONE',  ( -0.000000000000000000, -0.000000000000000000, 1.000000000000000000 ) ) ;
#11307 = UNCERTAINTY_MEASURE_WITH_UNIT (LENGTH_MEASURE( 1.000000000000000082E-05 ), #109, 'distance_accuracy_value', 'NONE');
#11308 = EDGE_LOOP ( 'NONE', ( #1549, #4089 ) ) ;
#11309 = AXIS2_PLACEMENT_3D ( 'NONE', #6281, #1823, #687 ) ;
#11310 = VERTEX_POINT ( 'NONE', #5969 ) ;
#11311 = DIRECTION ( 'NONE',  ( -1.000000000000000000, 0.000000000000000000, 0.000000000000000000 ) ) ;
#11312 = ORIENTED_EDGE ( 'NONE', *, *, #4407, .F. ) ;
#11313 = CARTESIAN_POINT ( 'NONE',  ( -1.059188295049996231, -6.027090492554000534, 7.250000000000000000 ) ) ;
#11314 = DIRECTION ( 'NONE',  ( 0.000000000000000000, 0.000000000000000000, 1.000000000000000000 ) ) ;
#11315 = CARTESIAN_POINT ( 'NONE',  ( 44.63563590245420443, 108.9054980190242503, 22.75000000000000000 ) ) ;
#11316 = ORIENTED_EDGE ( 'NONE', *, *, #13801, .F. ) ;
#11317 = CARTESIAN_POINT ( 'NONE',  ( -35.05918829505000645, 27.97290950744599769, 7.250000000000000000 ) ) ;
#11318 = EDGE_CURVE ( 'NONE', #10704, #4651, #5737, .T. ) ;
#11319 =( BOUNDED_CURVE ( )  B_SPLINE_CURVE ( 3, ( #4186, #6344, #7650, #5220 ),
 .UNSPECIFIED., .F., .F. ) 
 B_SPLINE_CURVE_WITH_KNOTS ( ( 4, 4 ),
 ( 1.570796326794896558, 3.141592653589793116 ),
 .UNSPECIFIED. ) 
 CURVE ( )  GEOMETRIC_REPRESENTATION_ITEM ( )  RATIONAL_B_SPLINE_CURVE ( ( 1.000000000000000000, 0.8047378541243649375, 0.8047378541243649375, 1.000000000000000000 ) ) 
 REPRESENTATION_ITEM ( '' )  );
#11320 = DIRECTION ( 'NONE',  ( -1.000000000000000000, 0.000000000000000000, 0.000000000000000000 ) ) ;
#11321 = CARTESIAN_POINT ( 'NONE',  ( 0.000000000000000000, 4.500000000000000000, 0.000000000000000000 ) ) ;
#11322 = ORIENTED_EDGE ( 'NONE', *, *, #982, .T. ) ;
#11323 = ORIENTED_EDGE ( 'NONE', *, *, #11053, .F. ) ;
#11324 = CARTESIAN_POINT ( 'NONE',  ( -14.81806704493275184, 30.13305483532533913, 55.03841218677168712 ) ) ;
#11325 = AXIS2_PLACEMENT_3D ( 'NONE', #12943, #561, #11183 ) ;
#11326 = CIRCLE ( 'NONE', #1092, 9.999999999999994671 ) ;
#11327 = ORIENTED_EDGE ( 'NONE', *, *, #6977, .F. ) ;
#11328 = ORIENTED_EDGE ( 'NONE', *, *, #2274, .T. ) ;
#11329 = VECTOR ( 'NONE', #5820, 1000.000000000000000 ) ;
#11330 = CARTESIAN_POINT ( 'NONE',  ( 109.6856792294029219, 115.9888905337886769, 19.25000000000000000 ) ) ;
#11331 = CYLINDRICAL_SURFACE ( 'NONE', #3379, 33.00000000000000000 ) ;
#11332 = VERTEX_POINT ( 'NONE', #9207 ) ;
#11333 = CARTESIAN_POINT ( 'NONE',  ( 100.2760581142613603, 115.9375248198690826, 20.00000000000000000 ) ) ;
#11334 = DIRECTION ( 'NONE',  ( 0.000000000000000000, 0.000000000000000000, -1.000000000000000000 ) ) ;
#11335 = EDGE_CURVE ( 'NONE', #6329, #5535, #7504, .T. ) ;
#11336 = CARTESIAN_POINT ( 'NONE',  ( -18.05918829504999934, 10.97290950744599947, 64.85000000000000853 ) ) ;
#11337 = DIRECTION ( 'NONE',  ( -0.000000000000000000, -0.000000000000000000, -1.000000000000000000 ) ) ;
#11338 = CARTESIAN_POINT ( 'NONE',  ( 68.49370948373500312, 123.0390816101113245, 0.7500000000000006661 ) ) ;
#11339 = CARTESIAN_POINT ( 'NONE',  ( 98.27605811426136029, 115.9375248198690826, 10.00000000000000000 ) ) ;
#11340 = AXIS2_PLACEMENT_3D ( 'NONE', #11458, #9775, #9567 ) ;
#11341 = TOROIDAL_SURFACE ( 'NONE', #11553, 10.75000000000000000, 0.7500000000000000000 ) ;
#11342 = VECTOR ( 'NONE', #8403, 1000.000000000000000 ) ;
#11343 = ADVANCED_FACE ( 'NONE', ( #13009 ), #3454, .F. ) ;
#11344 = EDGE_LOOP ( 'NONE', ( #8078, #2260, #12446, #1359 ) ) ;
#11345 = ORIENTED_EDGE ( 'NONE', *, *, #1714, .F. ) ;
#11346 = ORIENTED_EDGE ( 'NONE', *, *, #4794, .T. ) ;
#11347 = AXIS2_PLACEMENT_3D ( 'NONE', #4005, #4210, #10490 ) ;
#11348 = AXIS2_PLACEMENT_3D ( 'NONE', #9211, #609, #3074 ) ;
#11349 = LINE ( 'NONE', #7145, #11122 ) ;
#11350 = EDGE_CURVE ( 'NONE', #5154, #10379, #5079, .T. ) ;
#11351 = CIRCLE ( 'NONE', #7989, 4.750000000000000888 ) ;
#11352 = VERTEX_POINT ( 'NONE', #13077 ) ;
#11353 = CARTESIAN_POINT ( 'NONE',  ( 74.18094369249178044, 97.20665973629650125, 10.00000000000000000 ) ) ;
#11354 = DIRECTION ( 'NONE',  ( -1.000000000000000000, 0.000000000000000000, 0.000000000000000000 ) ) ;
#11355 = DIRECTION ( 'NONE',  ( 0.000000000000000000, 0.000000000000000000, 1.000000000000000000 ) ) ;
#11356 = CARTESIAN_POINT ( 'NONE',  ( -12.00000000000000000, 2.500000000000000000, -65.00000000000000000 ) ) ;
#11357 = CARTESIAN_POINT ( 'NONE',  ( -18.05918829504999934, 14.81548537210212046, 17.25000000000000000 ) ) ;
#11358 = PRODUCT_CONTEXT ( 'NONE', #9748, 'mechanical' ) ;
#11359 = ORIENTED_EDGE ( 'NONE', *, *, #9029, .T. ) ;
#11360 = EDGE_CURVE ( 'NONE', #5517, #6706, #10926, .T. ) ;
#11361 = AXIS2_PLACEMENT_3D ( 'NONE', #1187, #1328, #2122 ) ;
#11362 = AXIS2_PLACEMENT_3D ( 'NONE', #11984, #1370, #8985 ) ;
#11363 = CARTESIAN_POINT ( 'NONE',  ( -18.05918829504999934, 10.97290950744599947, 23.90000000000000213 ) ) ;
#11364 = CARTESIAN_POINT ( 'NONE',  ( 50.53208251186094202, 90.00905140961751272, 23.00000000000000000 ) ) ;
#11365 = DIRECTION ( 'NONE',  ( 0.000000000000000000, 0.000000000000000000, 1.000000000000000000 ) ) ;
#11366 = FACE_OUTER_BOUND ( 'NONE', #4849, .T. ) ;
#11367 = CARTESIAN_POINT ( 'NONE',  ( -23.05918829504999934, 10.97290950744599947, 68.84999999999999432 ) ) ;
#11368 = CARTESIAN_POINT ( 'NONE',  ( -23.33437236814141613, 12.98656286991741560, 68.21197126838345071 ) ) ;
#11369 = CARTESIAN_POINT ( 'NONE',  ( 134.8856359024541973, 90.15549801902423610, 23.00000000000000000 ) ) ;
#11370 = CARTESIAN_POINT ( 'NONE',  ( -9.640422211807251784, -16.89844320975769776, 0.000000000000000000 ) ) ;
#11371 = CARTESIAN_POINT ( 'NONE',  ( -25.73489962141544751, -4.139534227248430120, 57.35000000000000142 ) ) ;
#11372 = DIRECTION ( 'NONE',  ( 0.000000000000000000, 0.000000000000000000, -1.000000000000000000 ) ) ;
#11373 = CIRCLE ( 'NONE', #8016, 15.45000000000000462 ) ;
#11374 = CARTESIAN_POINT ( 'NONE',  ( -18.05918829504999934, 10.00028003023991907, 63.45000000000000284 ) ) ;
#11375 = AXIS2_PLACEMENT_3D ( 'NONE', #108, #4382, #6400 ) ;
#11376 = ADVANCED_FACE ( 'NONE', ( #2351 ), #4564, .F. ) ;
#11377 = EDGE_CURVE ( 'NONE', #7947, #7472, #1346, .T. ) ;
#11378 = ORIENTED_EDGE ( 'NONE', *, *, #11585, .F. ) ;
#11379 = FACE_OUTER_BOUND ( 'NONE', #2616, .T. ) ;
#11380 = VERTEX_POINT ( 'NONE', #11001 ) ;
#11381 = CARTESIAN_POINT ( 'NONE',  ( -20.90380367978140796, 15.13103491944108470, 68.81278884182248134 ) ) ;
#11382 = CARTESIAN_POINT ( 'NONE',  ( 140.3856359024541973, 108.6554980190242503, 23.00000000000000000 ) ) ;
#11383 = PRESENTATION_STYLE_ASSIGNMENT (( #12430 ) ) ;
#11384 = CARTESIAN_POINT ( 'NONE',  ( -18.05918829504999934, 19.07290950615085023, 63.35000000000700027 ) ) ;
#11385 = DIRECTION ( 'NONE',  ( 0.000000000000000000, 0.000000000000000000, 1.000000000000000000 ) ) ;
#11386 = CARTESIAN_POINT ( 'NONE',  ( 134.6356359024541973, 108.9054980190242503, 23.00000000000000000 ) ) ;
#11387 = CIRCLE ( 'NONE', #12282, 4.250000000000000000 ) ;
#11388 = CIRCLE ( 'NONE', #11611, 1.999999999999994893 ) ;
#11389 = AXIS2_PLACEMENT_3D ( 'NONE', #1119, #10701, #6228 ) ;
#11390 = EDGE_CURVE ( 'NONE', #12299, #9458, #8539, .T. ) ;
#11391 = ORIENTED_EDGE ( 'NONE', *, *, #9679, .F. ) ;
#11392 = EDGE_CURVE ( 'NONE', #9665, #6295, #3551, .T. ) ;
#11393 = ORIENTED_EDGE ( 'NONE', *, *, #9968, .T. ) ;
#11394 = CARTESIAN_POINT ( 'NONE',  ( -14.49027952043798351, 30.08448262670741968, 55.77701067917464428 ) ) ;
#11395 = ORIENTED_EDGE ( 'NONE', *, *, #7902, .F. ) ;
#11396 = ORIENTED_EDGE ( 'NONE', *, *, #8365, .F. ) ;
#11397 = EDGE_LOOP ( 'NONE', ( #9107, #13070, #10883, #6143 ) ) ;
#11398 = CIRCLE ( 'NONE', #11181, 2.700000000000001066 ) ;
#11399 = SHAPE_REPRESENTATION ( 'Base Mounting Plate', ( #6434 ), #6225 ) ;
#11400 = FILL_AREA_STYLE ('',( #8177 ) ) ;
#11401 = VECTOR ( 'NONE', #901, 1000.000000000000000 ) ;
#11402 = CARTESIAN_POINT ( 'NONE',  ( -18.05918829505000289, 3.354823934416959919, 61.65955166408550525 ) ) ;
#11403 = VECTOR ( 'NONE', #9118, 1000.000000000000000 ) ;
#11404 = EDGE_LOOP ( 'NONE', ( #11816, #5047, #436, #8765 ) ) ;
#11405 = FACE_OUTER_BOUND ( 'NONE', #7124, .T. ) ;
#11406 = CARTESIAN_POINT ( 'NONE',  ( -23.49332020752115113, 0.2738342970428629952, 61.85000000000000142 ) ) ;
#11407 = FACE_OUTER_BOUND ( 'NONE', #10015, .T. ) ;
#11408 = CARTESIAN_POINT ( 'NONE',  ( -18.05918829504999934, 10.97290950744599947, 57.35000000000000142 ) ) ;
#11409 = CARTESIAN_POINT ( 'NONE',  ( -19.55892036123722022, 27.90662746311071629, 57.54959831248249458 ) ) ;
#11410 = CARTESIAN_POINT ( 'NONE',  ( -11.30918829504999934, 10.97290950744599947, 63.35000000000000142 ) ) ;
#11411 = VECTOR ( 'NONE', #13709, 1000.000000000000000 ) ;
#11412 = AXIS2_PLACEMENT_3D ( 'NONE', #4098, #7149, #6164 ) ;
#11413 = ORIENTED_EDGE ( 'NONE', *, *, #1714, .T. ) ;
#11414 = ORIENTED_EDGE ( 'NONE', *, *, #9253, .T. ) ;
#11415 = EDGE_CURVE ( 'NONE', #3674, #5251, #5522, .T. ) ;
#11416 = ORIENTED_EDGE ( 'NONE', *, *, #8796, .T. ) ;
#11417 = ORIENTED_EDGE ( 'NONE', *, *, #10459, .F. ) ;
#11418 = ORIENTED_EDGE ( 'NONE', *, *, #5686, .T. ) ;
#11419 = FACE_BOUND ( 'NONE', #8516, .T. ) ;
#11420 = ADVANCED_FACE ( 'NONE', ( #7537 ), #231, .T. ) ;
#11421 = CARTESIAN_POINT ( 'NONE',  ( -20.28447066877352611, 30.25344248482696585, 60.89002542176228872 ) ) ;
#11422 = AXIS2_PLACEMENT_3D ( 'NONE', #10057, #1386, #7722 ) ;
#11423 = CARTESIAN_POINT ( 'NONE',  ( -18.05918829504999934, 10.97290950744599947, 68.84999999999999432 ) ) ;
#11424 = DIRECTION ( 'NONE',  ( 0.000000000000000000, 1.000000000000000000, 2.202823461557851130E-15 ) ) ;
#11425 = CARTESIAN_POINT ( 'NONE',  ( 44.63563590245420443, 94.90549801902425031, 20.00000000000000000 ) ) ;
#11426 = LINE ( 'NONE', #10249, #11825 ) ;
#11427 = ADVANCED_FACE ( 'NONE', ( #2492 ), #1199, .T. ) ;
#11428 = AXIS2_PLACEMENT_3D ( 'NONE', #11501, #5006, #7164 ) ;
#11429 = LINE ( 'NONE', #13583, #6377 ) ;
#11430 = ORIENTED_EDGE ( 'NONE', *, *, #489, .F. ) ;
#11431 = EDGE_LOOP ( 'NONE', ( #13198, #2333, #11121, #10943 ) ) ;
#11432 = DIRECTION ( 'NONE',  ( -1.000000000000000000, 1.799713116287177675E-15, 0.000000000000000000 ) ) ;
#11433 = DIRECTION ( 'NONE',  ( -2.267612386897784912E-16, 1.000000000000000000, 0.000000000000000000 ) ) ;
#11434 = EDGE_CURVE ( 'NONE', #2075, #7909, #4498, .T. ) ;
#11435 = LINE ( 'NONE', #10454, #11182 ) ;
#11436 = CARTESIAN_POINT ( 'NONE',  ( -23.64255140084592099, 12.71465888092544638, 68.00600096910662273 ) ) ;
#11437 = CARTESIAN_POINT ( 'NONE',  ( -21.69796668809184936, 15.09714177616359798, 30.59999999999999787 ) ) ;
#11438 = DIRECTION ( 'NONE',  ( -0.000000000000000000, -0.000000000000000000, 1.000000000000000000 ) ) ;
#11439 = LINE ( 'NONE', #1879, #7361 ) ;
#11440 = AXIS2_PLACEMENT_3D ( 'NONE', #6320, #4302, #6162 ) ;
#11441 = CARTESIAN_POINT ( 'NONE',  ( -34.72201093190195564, 10.97290950744599947, 5.250000000000000000 ) ) ;
#11442 = FACE_BOUND ( 'NONE', #5694, .T. ) ;
#11443 = ORIENTED_EDGE ( 'NONE', *, *, #12847, .F. ) ;
#11444 = UNCERTAINTY_MEASURE_WITH_UNIT (LENGTH_MEASURE( 1.000000000000000082E-05 ), #4996, 'distance_accuracy_value', 'NONE');
#11445 = EDGE_CURVE ( 'NONE', #1998, #3512, #10446, .T. ) ;
#11446 = VERTEX_POINT ( 'NONE', #6647 ) ;
#11447 = AXIS2_PLACEMENT_3D ( 'NONE', #11941, #4009, #5113 ) ;
#11448 = CARTESIAN_POINT ( 'NONE',  ( -18.05918829504999934, 10.97290950744599947, 6.250000000000000000 ) ) ;
#11449 = VERTEX_POINT ( 'NONE', #7759 ) ;
#11450 = EDGE_LOOP ( 'NONE', ( #5263, #12365, #5144, #11749, #216, #6831, #5855, #3945, #2783, #10430, #12995, #6844, #2623, #7626 ) ) ;
#11451 = FACE_OUTER_BOUND ( 'NONE', #9009, .T. ) ;
#11452 = EDGE_CURVE ( 'NONE', #918, #13546, #9593, .T. ) ;
#11453 = CARTESIAN_POINT ( 'NONE',  ( -25.73489962141550080, -4.139534227248430120, 60.85000000000000142 ) ) ;
#11454 = DIRECTION ( 'NONE',  ( 0.000000000000000000, 0.000000000000000000, -1.000000000000000000 ) ) ;
#11455 = EDGE_CURVE ( 'NONE', #9940, #11194, #2669, .T. ) ;
#11456 = VERTEX_POINT ( 'NONE', #148 ) ;
#11457 = CARTESIAN_POINT ( 'NONE',  ( -1.859188294733151059, 19.07290950803865215, 63.35000000001166143 ) ) ;
#11458 = CARTESIAN_POINT ( 'NONE',  ( -1.059188295049996231, -6.027090492554000534, 68.85549045786049760 ) ) ;
#11459 = CARTESIAN_POINT ( 'NONE',  ( 92.63563590245421153, 85.78908161011133870, 0.000000000000000000 ) ) ;
#11460 = CIRCLE ( 'NONE', #9007, 16.50000000000000000 ) ;
#11461 = ORIENTED_EDGE ( 'NONE', *, *, #12687, .T. ) ;
#11462 = CARTESIAN_POINT ( 'NONE',  ( -15.59946857746960447, 30.22967062530674909, 60.68251737619485198 ) ) ;
#11463 = ORIENTED_EDGE ( 'NONE', *, *, #7012, .F. ) ;
#11464 = CARTESIAN_POINT ( 'NONE',  ( -18.05918829504999934, 10.97290950744599947, 64.85000000000000853 ) ) ;
#11465 = CARTESIAN_POINT ( 'NONE',  ( -5.640422211807260666, -16.89844320975769776, -3.000000000000000000 ) ) ;
#11466 = DIRECTION ( 'NONE',  ( -1.000000000000000000, 0.000000000000000000, 0.000000000000000000 ) ) ;
#11467 = VERTEX_POINT ( 'NONE', #11752 ) ;
#11468 = VERTEX_POINT ( 'NONE', #2205 ) ;
#11469 = CARTESIAN_POINT ( 'NONE',  ( -35.05918829505000645, 27.97290950744599769, 7.250000000000000000 ) ) ;
#11470 = FACE_BOUND ( 'NONE', #7717, .T. ) ;
#11471 = LINE ( 'NONE', #8184, #2491 ) ;
#11472 = LINE ( 'NONE', #7196, #11242 ) ;
#11473 = ORIENTED_EDGE ( 'NONE', *, *, #2498, .T. ) ;
#11474 = LINE ( 'NONE', #10299, #10268 ) ;
#11475 = EDGE_CURVE ( 'NONE', #4563, #3000, #6446, .T. ) ;
#11476 = CARTESIAN_POINT ( 'NONE',  ( -5.789834139046009298, 27.54455229823479812, 64.85000000000000853 ) ) ;
#11477 = ORIENTED_EDGE ( 'NONE', *, *, #12293, .T. ) ;
#11478 = EDGE_LOOP ( 'NONE', ( #5868, #2022, #11061, #9299 ) ) ;
#11479 = VERTEX_POINT ( 'NONE', #6517 ) ;
#11480 = ORIENTED_EDGE ( 'NONE', *, *, #2138, .F. ) ;
#11481 = CARTESIAN_POINT ( 'NONE',  ( -3.499999999999998224, 2.000000000000000000, -65.00000000000000000 ) ) ;
#11482 = CARTESIAN_POINT ( 'NONE',  ( -20.15923745082466567, 30.26546654931225788, 60.99209064090569399 ) ) ;
#11483 = CARTESIAN_POINT ( 'NONE',  ( 27.50000000000001066, 9.000000000000000000, 29.99999999999999645 ) ) ;
#11484 = LINE ( 'NONE', #10437, #10881 ) ;
#11485 = DIRECTION ( 'NONE',  ( 1.000000000000000000, 0.000000000000000000, 0.000000000000000000 ) ) ;
#11486 = EDGE_CURVE ( 'NONE', #2900, #5058, #4883, .T. ) ;
#11487 = AXIS2_PLACEMENT_3D ( 'NONE', #10633, #144, #1056 ) ;
#11488 = CYLINDRICAL_SURFACE ( 'NONE', #8930, 24.92993838181874722 ) ;
#11489 = SHAPE_DEFINITION_REPRESENTATION ( #6529, #11848 ) ;
#11490 = VERTEX_POINT ( 'NONE', #6993 ) ;
#11491 = CLOSED_SHELL ( 'NONE', ( #2655, #11863, #6730, #9792, #6797, #9041, #9018, #8502, #12189, #1036, #12136, #11599, #10658, #11302, #6859, #3639, #186, #6190, #9084, #663, #6437, #13088, #13150, #5626, #4167, #12882, #10508 ) ) ;
#11492 = EDGE_CURVE ( 'NONE', #10592, #9008, #7097, .T. ) ;
#11493 = EDGE_LOOP ( 'NONE', ( #13720, #3346 ) ) ;
#11494 = AXIS2_PLACEMENT_3D ( 'NONE', #5281, #2383, #9558 ) ;
#11495 = CARTESIAN_POINT ( 'NONE',  ( 140.6356359024541973, 113.0390816101113387, 0.3106601717798218587 ) ) ;
#11496 = CARTESIAN_POINT ( 'NONE',  ( -7.241070169793063727, -7.867426463707971607, 83.57661607529820458 ) ) ;
#11497 = ORIENTED_EDGE ( 'NONE', *, *, #3497, .F. ) ;
#11498 = DIRECTION ( 'NONE',  ( 0.000000000000000000, 0.000000000000000000, 1.000000000000000000 ) ) ;
#11499 = DIRECTION ( 'NONE',  ( 1.000000000000000000, 0.000000000000000000, 0.000000000000000000 ) ) ;
#11500 = CARTESIAN_POINT ( 'NONE',  ( 134.6356359024541973, 94.90549801902425031, 23.00000000000000000 ) ) ;
#11501 = CARTESIAN_POINT ( 'NONE',  ( -18.05918829504999934, 10.97290950744599947, 27.09999999999999787 ) ) ;
#11502 = CARTESIAN_POINT ( 'NONE',  ( 134.6356359024541973, 89.90549801902423610, 22.75000000000000000 ) ) ;
#11503 = CARTESIAN_POINT ( 'NONE',  ( 0.04028432657539327000, 4.500000000000000000, -16.54539866546729954 ) ) ;
#11504 = DIRECTION ( 'NONE',  ( 0.000000000000000000, 0.000000000000000000, -1.000000000000000000 ) ) ;
#11505 = ADVANCED_FACE ( 'NONE', ( #13223 ), #6788, .T. ) ;
#11506 = PLANE ( 'NONE',  #13682 ) ;
#11507 = DIRECTION ( 'NONE',  ( -0.000000000000000000, -0.000000000000000000, -1.000000000000000000 ) ) ;
#11508 = ORIENTED_EDGE ( 'NONE', *, *, #4814, .F. ) ;
#11509 = CIRCLE ( 'NONE', #8826, 6.849999999999999645 ) ;
#11510 = ORIENTED_EDGE ( 'NONE', *, *, #5344, .F. ) ;
#11511 = ADVANCED_FACE ( 'NONE', ( #7056 ), #13284, .F. ) ;
#11512 = ORIENTED_EDGE ( 'NONE', *, *, #1244, .T. ) ;
#11513 = CARTESIAN_POINT ( 'NONE',  ( 3.690811704950004657, -6.027090492554000534, 7.250000000000000000 ) ) ;
#11514 = VERTEX_POINT ( 'NONE', #4711 ) ;
#11515 = ORIENTED_EDGE ( 'NONE', *, *, #3666, .F. ) ;
#11516 = CARTESIAN_POINT ( 'NONE',  ( -20.60782847033100040, 15.39217156908933859, 68.75034594041223102 ) ) ;
#11517 = CARTESIAN_POINT ( 'NONE',  ( -12.81426999815532497, 15.06602133594271820, 7.000000000000000000 ) ) ;
#11518 = DIRECTION ( 'NONE',  ( 0.000000000000000000, 0.000000000000000000, 1.000000000000000000 ) ) ;
#11519 = DIRECTION ( 'NONE',  ( 0.000000000000000000, 1.000000000000000000, 0.000000000000000000 ) ) ;
#11520 = EDGE_CURVE ( 'NONE', #9971, #1130, #13780, .T. ) ;
#11521 = DIRECTION ( 'NONE',  ( 0.000000000000000000, 0.000000000000000000, 1.000000000000000000 ) ) ;
#11522 = CIRCLE ( 'NONE', #13531, 3.000000000000002665 ) ;
#11523 = ADVANCED_FACE ( 'NONE', ( #4910 ), #4835, .T. ) ;
#11524 = EDGE_LOOP ( 'NONE', ( #2130, #7159 ) ) ;
#11525 = CARTESIAN_POINT ( 'NONE',  ( -14.34316551184594424, 30.06124217888930872, 56.29137106245990196 ) ) ;
#11526 = EDGE_LOOP ( 'NONE', ( #10010, #325, #8175, #13500 ) ) ;
#11527 = ORIENTED_EDGE ( 'NONE', *, *, #5186, .F. ) ;
#11528 = ORIENTED_EDGE ( 'NONE', *, *, #12030, .F. ) ;
#11529 = CARTESIAN_POINT ( 'NONE',  ( -38.05918829505000645, 27.97290950744599769, 0.000000000000000000 ) ) ;
#11530 = CARTESIAN_POINT ( 'NONE',  ( -23.42001676333060090, -4.028726038184999858, 63.45000000000000284 ) ) ;
#11531 = AXIS2_PLACEMENT_3D ( 'NONE', #3830, #12879, #9683 ) ;
#11532 = DIRECTION ( 'NONE',  ( 1.000000000000000000, 0.000000000000000000, 0.000000000000000000 ) ) ;
#11533 = EDGE_LOOP ( 'NONE', ( #13124, #4330, #7969, #11932 ) ) ;
#11534 = CARTESIAN_POINT ( 'NONE',  ( 0.04028432657539327000, 4.500000000000000000, -18.54539866546729243 ) ) ;
#11535 = CYLINDRICAL_SURFACE ( 'NONE', #13573, 0.7499999999999973355 ) ;
#11536 = AXIS2_PLACEMENT_3D ( 'NONE', #11999, #11031, #4741 ) ;
#11537 = FACE_OUTER_BOUND ( 'NONE', #23, .T. ) ;
#11538 = DIRECTION ( 'NONE',  ( 0.4528443260392608916, 0.8915896008669279560, 0.000000000000000000 ) ) ;
#11539 = CARTESIAN_POINT ( 'NONE',  ( -17.66997072932066359, 27.96944788186879194, 58.81217888752696155 ) ) ;
#11540 = PLANE ( 'NONE',  #12507 ) ;
#11541 = AXIS2_PLACEMENT_3D ( 'NONE', #6381, #5394, #6321 ) ;
#11542 = ORIENTED_EDGE ( 'NONE', *, *, #3991, .F. ) ;
#11543 = AXIS2_PLACEMENT_3D ( 'NONE', #590, #10365, #4922 ) ;
#11544 = VERTEX_POINT ( 'NONE', #3664 ) ;
#11545 = ADVANCED_FACE ( 'NONE', ( #3722 ), #13269, .F. ) ;
#11546 = ORIENTED_EDGE ( 'NONE', *, *, #3572, .T. ) ;
#11547 = CARTESIAN_POINT ( 'NONE',  ( 6.940811704950009542, -11.02709049255400053, 10.00000000000000000 ) ) ;
#11548 = CARTESIAN_POINT ( 'NONE',  ( -18.05918829504999934, 10.97290950744599947, 61.86500000000000199 ) ) ;
#11549 = ORIENTED_EDGE ( 'NONE', *, *, #10067, .F. ) ;
#11550 = CARTESIAN_POINT ( 'NONE',  ( -18.96245718805280944, 30.34273348207711507, 61.58489515985737484 ) ) ;
#11551 = VECTOR ( 'NONE', #7660, 1000.000000000000000 ) ;
#11552 = CARTESIAN_POINT ( 'NONE',  ( -18.93945023811382455, 26.94867995574305297, 56.13543987128847590 ) ) ;
#11553 = AXIS2_PLACEMENT_3D ( 'NONE', #2004, #940, #1723 ) ;
#11554 = CARTESIAN_POINT ( 'NONE',  ( -25.33503448090910126, 29.19143287883919768, 64.85000000000000853 ) ) ;
#11555 = CARTESIAN_POINT ( 'NONE',  ( -9.640422211807251784, -16.89844320975769776, -3.000000000000000000 ) ) ;
#11556 = AXIS2_PLACEMENT_3D ( 'NONE', #1134, #2282, #6519 ) ;
#11557 = PLANE ( 'NONE',  #10941 ) ;
#11558 = PRODUCT_CONTEXT ( 'NONE', #1443, 'mechanical' ) ;
#11559 = ORIENTED_EDGE ( 'NONE', *, *, #10936, .F. ) ;
#11560 = ADVANCED_FACE ( 'NONE', ( #12243 ), #2699, .T. ) ;
#11561 = AXIS2_PLACEMENT_3D ( 'NONE', #3432, #7770, #10895 ) ;
#11562 = EDGE_CURVE ( 'NONE', #2919, #9409, #13127, .T. ) ;
#11563 = VECTOR ( 'NONE', #7601, 1000.000000000000000 ) ;
#11564 = AXIS2_PLACEMENT_3D ( 'NONE', #3226, #10821, #3161 ) ;
#11565 = ORIENTED_EDGE ( 'NONE', *, *, #828, .T. ) ;
#11566 = EDGE_CURVE ( 'NONE', #11864, #12408, #7511, .T. ) ;
#11567 = VECTOR ( 'NONE', #8086, 1000.000000000000114 ) ;
#11568 = CARTESIAN_POINT ( 'NONE',  ( 140.5069562460138286, 112.7284214383315089, 20.00000000000000000 ) ) ;
#11569 = DIRECTION ( 'NONE',  ( 1.000000000000000000, 0.000000000000000000, 0.000000000000000000 ) ) ;
#11570 = EDGE_CURVE ( 'NONE', #1264, #13079, #5090, .T. ) ;
#11571 = ORIENTED_EDGE ( 'NONE', *, *, #2571, .F. ) ;
#11572 = CYLINDRICAL_SURFACE ( 'NONE', #1814, 1.999999999999991340 ) ;
#11573 = DIRECTION ( 'NONE',  ( -1.000000000000000000, 0.000000000000000000, 0.000000000000000000 ) ) ;
#11574 = DIRECTION ( 'NONE',  ( 0.000000000000000000, 0.000000000000000000, 1.000000000000000000 ) ) ;
#11575 = FACE_OUTER_BOUND ( 'NONE', #724, .T. ) ;
#11576 = DIRECTION ( 'NONE',  ( 0.000000000000000000, 0.000000000000000000, 1.000000000000000000 ) ) ;
#11577 = CARTESIAN_POINT ( 'NONE',  ( 24.03999999999999915, 2.944050905150237001E-15, 7.000000000000000000 ) ) ;
#11578 = CARTESIAN_POINT ( 'NONE',  ( 18.45469220996244886, 1.832421873814834123, -3.000000000000000000 ) ) ;
#11579 = FACE_OUTER_BOUND ( 'NONE', #5436, .T. ) ;
#11580 = AXIS2_PLACEMENT_3D ( 'NONE', #11374, #5076, #2947 ) ;
#11581 = VECTOR ( 'NONE', #3295, 1000.000000000000000 ) ;
#11582 = VECTOR ( 'NONE', #2375, 1000.000000000000000 ) ;
#11583 = CONICAL_SURFACE ( 'NONE', #12029, 4.250000000000000000, 0.7853981633974518317 ) ;
#11584 = ORIENTED_EDGE ( 'NONE', *, *, #13603, .T. ) ;
#11585 = EDGE_CURVE ( 'NONE', #9992, #363, #10013, .T. ) ;
#11586 = CARTESIAN_POINT ( 'NONE',  ( -4.599650328638321461, 0.000000000000000000, -7.878124499050794149 ) ) ;
#11587 = EDGE_CURVE ( 'NONE', #2353, #9556, #5528, .T. ) ;
#11588 = VERTEX_POINT ( 'NONE', #514 ) ;
#11589 = DIRECTION ( 'NONE',  ( -1.000000000000000000, 0.000000000000000000, 0.000000000000000000 ) ) ;
#11590 = EDGE_LOOP ( 'NONE', ( #8338, #7708, #6230, #3535 ) ) ;
#11591 = EDGE_CURVE ( 'NONE', #2653, #12520, #10683, .T. ) ;
#11592 = CARTESIAN_POINT ( 'NONE',  ( -6.000000000000000888, 11.99999999999999822, 7.000000000000000000 ) ) ;
#11593 = LINE ( 'NONE', #9227, #9784 ) ;
#11594 = EDGE_CURVE ( 'NONE', #1667, #803, #7125, .T. ) ;
#11595 = DIRECTION ( 'NONE',  ( 1.000000000000000000, 0.000000000000000000, -0.000000000000000000 ) ) ;
#11596 = AXIS2_PLACEMENT_3D ( 'NONE', #2612, #10143, #10081 ) ;
#11597 = CIRCLE ( 'NONE', #6016, 34.69999999999999574 ) ;
#11598 = EDGE_LOOP ( 'NONE', ( #4103, #6157, #4088, #11477 ) ) ;
#11599 = ADVANCED_FACE ( 'NONE', ( #13492 ), #5110, .F. ) ;
#11600 = CARTESIAN_POINT ( 'NONE',  ( -14.49575039789787390, 30.08533272846046813, 58.93884046276453148 ) ) ;
#11601 = EDGE_LOOP ( 'NONE', ( #13470, #11797, #10869, #13708 ) ) ;
#11602 = PLANE ( 'NONE',  #6151 ) ;
#11603 = ADVANCED_FACE ( 'NONE', ( #6303 ), #7253, .T. ) ;
#11604 = DIRECTION ( 'NONE',  ( 0.000000000000000000, -1.000000000000000000, 0.000000000000000000 ) ) ;
#11605 = EDGE_LOOP ( 'NONE', ( #9636, #10304, #65, #909 ) ) ;
#11606 = FACE_OUTER_BOUND ( 'NONE', #12670, .T. ) ;
#11607 = CYLINDRICAL_SURFACE ( 'NONE', #10242, 34.69999999999999574 ) ;
#11608 = EDGE_CURVE ( 'NONE', #13266, #6817, #4215, .T. ) ;
#11609 = CARTESIAN_POINT ( 'NONE',  ( 0.04028432657539351286, 4.500000000000000000, -20.54539866546728533 ) ) ;
#11610 = CONICAL_SURFACE ( 'NONE', #6913, 6.850000000000002309, 0.7853981633974433940 ) ;
#11611 = AXIS2_PLACEMENT_3D ( 'NONE', #5858, #621, #10072 ) ;
#11612 = VECTOR ( 'NONE', #6244, 1000.000000000000000 ) ;
#11613 = CIRCLE ( 'NONE', #466, 7.618085573000000110 ) ;
#11614 = CARTESIAN_POINT ( 'NONE',  ( 140.6356359024541973, 113.0390816101113387, 20.00000000000000000 ) ) ;
#11615 = DIRECTION ( 'NONE',  ( 0.000000000000000000, 0.000000000000000000, -1.000000000000000000 ) ) ;
#11616 = ORIENTED_EDGE ( 'NONE', *, *, #7980, .T. ) ;
#11617 = ORIENTED_EDGE ( 'NONE', *, *, #12028, .F. ) ;
#11618 = CIRCLE ( 'NONE', #13397, 0.7500000000000000000 ) ;
#11619 = AXIS2_PLACEMENT_3D ( 'NONE', #4267, #11871, #7583 ) ;
#11620 = AXIS2_PLACEMENT_3D ( 'NONE', #12964, #2232, #2376 ) ;
#11621 = VERTEX_POINT ( 'NONE', #9377 ) ;
#11622 = VERTEX_POINT ( 'NONE', #6010 ) ;
#11623 = ORIENTED_EDGE ( 'NONE', *, *, #10775, .T. ) ;
#11624 = DIRECTION ( 'NONE',  ( 0.000000000000000000, 0.000000000000000000, -1.000000000000000000 ) ) ;
#11625 = CARTESIAN_POINT ( 'NONE',  ( -35.05918829505000645, -6.027090492554000534, 5.250000000000000000 ) ) ;
#11626 = ORIENTED_EDGE ( 'NONE', *, *, #7645, .F. ) ;
#11627 = ADVANCED_FACE ( 'NONE', ( #11606 ), #7325, .F. ) ;
#11628 = LINE ( 'NONE', #8608, #13412 ) ;
#11629 = CARTESIAN_POINT ( 'NONE',  ( -17.92868857854553610, 26.97291705118750116, 55.84994910580621763 ) ) ;
#11630 = CARTESIAN_POINT ( 'NONE',  ( -35.05918829505000645, -6.027090492554000534, 0.000000000000000000 ) ) ;
#11631 = DIRECTION ( 'NONE',  ( 0.000000000000000000, 0.000000000000000000, 1.000000000000000000 ) ) ;
#11632 = FACE_OUTER_BOUND ( 'NONE', #7235, .T. ) ;
#11633 = CIRCLE ( 'NONE', #12749, 6.450000000000001066 ) ;
#11634 = AXIS2_PLACEMENT_3D ( 'NONE', #8696, #12819, #10872 ) ;
#11635 = ORIENTED_EDGE ( 'NONE', *, *, #3826, .F. ) ;
#11636 = AXIS2_PLACEMENT_3D ( 'NONE', #11146, #12056, #11082 ) ;
#11637 = B_SPLINE_CURVE_WITH_KNOTS ( 'NONE', 3,
 ( #7767, #13290, #7838, #10935 ),
 .UNSPECIFIED., .F., .F.,
 ( 4, 4 ),
 ( 0.000000000000000000, 1.000000000000000000 ),
 .UNSPECIFIED. ) ;
#11638 = VERTEX_POINT ( 'NONE', #8326 ) ;
#11639 = VERTEX_POINT ( 'NONE', #12656 ) ;
#11640 = CONICAL_SURFACE ( 'NONE', #12755, 2.800000000000000266, 0.7853981633974419507 ) ;
#11641 = DIRECTION ( 'NONE',  ( -0.000000000000000000, -0.000000000000000000, 1.000000000000000000 ) ) ;
#11642 = AXIS2_PLACEMENT_3D ( 'NONE', #6650, #13226, #2495 ) ;
#11643 = CARTESIAN_POINT ( 'NONE',  ( 0.000000000000000000, 4.500000000000000000, -23.49999999999999645 ) ) ;
#11644 = CIRCLE ( 'NONE', #1116, 1.999999999999991340 ) ;
#11645 = VERTEX_POINT ( 'NONE', #5035 ) ;
#11646 = FACE_OUTER_BOUND ( 'NONE', #10135, .T. ) ;
#11647 = CARTESIAN_POINT ( 'NONE',  ( 140.3249757306743675, 85.78908161011133870, 20.00000000000000000 ) ) ;
#11648 = CARTESIAN_POINT ( 'NONE',  ( 5.640422211807141650, 16.89844320975774750, -3.000000000000000000 ) ) ;
#11649 = EDGE_CURVE ( 'NONE', #3543, #209, #11119, .T. ) ;
#11650 = DIRECTION ( 'NONE',  ( 1.000000000000000000, 0.000000000000000000, 0.000000000000000000 ) ) ;
#11651 = DIRECTION ( 'NONE',  ( -0.000000000000000000, 1.000000000000000000, -0.000000000000000000 ) ) ;
#11652 = FACE_OUTER_BOUND ( 'NONE', #9845, .T. ) ;
#11653 = DIRECTION ( 'NONE',  ( 0.000000000000000000, -1.000000000000000000, 0.000000000000000000 ) ) ;
#11654 = CARTESIAN_POINT ( 'NONE',  ( 0.000000000000000000, 0.000000000000000000, 0.000000000000000000 ) ) ;
#11655 = ADVANCED_FACE ( 'NONE', ( #10562 ), #2904, .F. ) ;
#11656 = EDGE_CURVE ( 'NONE', #2349, #2553, #6078, .T. ) ;
#11657 = AXIS2_PLACEMENT_3D ( 'NONE', #9420, #8358, #9618 ) ;
#11658 = ORIENTED_EDGE ( 'NONE', *, *, #9411, .F. ) ;
#11659 = EDGE_LOOP ( 'NONE', ( #4770, #12600, #11176, #10320 ) ) ;
#11660 = CARTESIAN_POINT ( 'NONE',  ( -10.25088531517542023, -8.860076549334110041, 17.25000000000000000 ) ) ;
#11661 = ORIENTED_EDGE ( 'NONE', *, *, #2309, .T. ) ;
#11662 = ORIENTED_EDGE ( 'NONE', *, *, #9984, .F. ) ;
#11663 = EDGE_LOOP ( 'NONE', ( #1623, #8006, #11549, #2118, #6020 ) ) ;
#11664 = CARTESIAN_POINT ( 'NONE',  ( -13.12714905285830547, 8.656502101311028596, 68.40310675162322696 ) ) ;
#11665 = ORIENTED_EDGE ( 'NONE', *, *, #7858, .F. ) ;
#11666 = DIRECTION ( 'NONE',  ( 1.000000000000000000, 0.000000000000000000, 0.000000000000000000 ) ) ;
#11667 = DIRECTION ( 'NONE',  ( 0.000000000000000000, -1.000000000000000000, 0.000000000000000000 ) ) ;
#11668 = ORIENTED_EDGE ( 'NONE', *, *, #5532, .T. ) ;
#11669 = CARTESIAN_POINT ( 'NONE',  ( -15.99409762314761885, 6.127015440082126396, 68.58244592664642880 ) ) ;
#11670 = DIRECTION ( 'NONE',  ( 0.000000000000000000, 0.000000000000000000, 1.000000000000000000 ) ) ;
#11671 = EDGE_CURVE ( 'NONE', #2036, #7771, #8455, .T. ) ;
#11672 = CIRCLE ( 'NONE', #5202, 1.725000000000000755 ) ;
#11673 = CARTESIAN_POINT ( 'NONE',  ( -15.27301918356318033, 30.19258199384825403, 54.36937504594504134 ) ) ;
#11674 = VERTEX_POINT ( 'NONE', #5239 ) ;
#11675 = VERTEX_POINT ( 'NONE', #9509 ) ;
#11676 = VERTEX_POINT ( 'NONE', #7191 ) ;
#11677 = DIRECTION ( 'NONE',  ( 0.7071067811865525687, 0.7071067811865425767, -0.000000000000000000 ) ) ;
#11678 = DIRECTION ( 'NONE',  ( -0.000000000000000000, -0.000000000000000000, -1.000000000000000000 ) ) ;
#11679 = CARTESIAN_POINT ( 'NONE',  ( -1.059188295049996231, -6.027090492554000534, 17.25000000000000000 ) ) ;
#11680 = FACE_OUTER_BOUND ( 'NONE', #5931, .T. ) ;
#11681 = FACE_OUTER_BOUND ( 'NONE', #8885, .T. ) ;
#11682 = CIRCLE ( 'NONE', #3217, 1.999999999999993117 ) ;
#11683 = DIRECTION ( 'NONE',  ( 0.000000000000000000, 0.000000000000000000, 1.000000000000000000 ) ) ;
#11684 = ADVANCED_FACE ( 'NONE', ( #11405 ), #12233, .T. ) ;
#11685 = DIRECTION ( 'NONE',  ( 0.000000000000000000, 0.000000000000000000, -1.000000000000000000 ) ) ;
#11686 = ORIENTED_EDGE ( 'NONE', *, *, #13401, .F. ) ;
#11687 = EDGE_LOOP ( 'NONE', ( #8799, #5282, #760, #2070 ) ) ;
#11688 = ADVANCED_FACE ( 'NONE', ( #10353 ), #6200, .F. ) ;
#11689 = EDGE_LOOP ( 'NONE', ( #935, #10289, #5521, #8824 ) ) ;
#11690 = ORIENTED_EDGE ( 'NONE', *, *, #4768, .T. ) ;
#11691 = ORIENTED_EDGE ( 'NONE', *, *, #5984, .T. ) ;
#11692 = ORIENTED_EDGE ( 'NONE', *, *, #4254, .T. ) ;
#11693 = CARTESIAN_POINT ( 'NONE',  ( -8.930582367738718830, 12.35910059330153921, 64.85000000000000853 ) ) ;
#11694 = DIRECTION ( 'NONE',  ( 0.000000000000000000, 0.000000000000000000, -1.000000000000000000 ) ) ;
#11695 = ORIENTED_EDGE ( 'NONE', *, *, #5785, .F. ) ;
#11696 = DIRECTION ( 'NONE',  ( -0.2878798879079283446, 0.9576665234506834823, 0.000000000000000000 ) ) ;
#11697 = DIRECTION ( 'NONE',  ( 1.000000000000000000, 0.000000000000000000, 0.000000000000000000 ) ) ;
#11698 = FACE_OUTER_BOUND ( 'NONE', #10442, .T. ) ;
#11699 = CARTESIAN_POINT ( 'NONE',  ( -43.05918829505001355, -11.02709049255400053, 10.00000000000000000 ) ) ;
#11700 = EDGE_CURVE ( 'NONE', #11290, #4952, #5311, .T. ) ;
#11701 = CARTESIAN_POINT ( 'NONE',  ( -1.059188295049996231, -6.027090492554000534, 64.85000000000000853 ) ) ;
#11702 = CONTEXT_DEPENDENT_SHAPE_REPRESENTATION ( #4574, #11824 ) ;
#11703 = ORIENTED_EDGE ( 'NONE', *, *, #12185, .F. ) ;
#11704 = EDGE_CURVE ( 'NONE', #13581, #5483, #2211, .T. ) ;
#11705 = EDGE_LOOP ( 'NONE', ( #6356, #2335, #9505, #4560, #6626, #3457, #5958, #11127 ) ) ;
#11706 = CARTESIAN_POINT ( 'NONE',  ( -25.32001676333059947, -4.028726038184999858, 62.14999999999999858 ) ) ;
#11707 = ORIENTED_EDGE ( 'NONE', *, *, #10700, .F. ) ;
#11708 = PLANE ( 'NONE',  #10477 ) ;
#11709 = CARTESIAN_POINT ( 'NONE',  ( -3.499999999999998224, 2.000000000000000000, 0.000000000000000000 ) ) ;
#11710 = CIRCLE ( 'NONE', #7015, 3.000000000000001332 ) ;
#11711 = CARTESIAN_POINT ( 'NONE',  ( -20.64360816717656988, 30.21612105584335595, 54.14118912831367680 ) ) ;
#11712 = CARTESIAN_POINT ( 'NONE',  ( -0.04028432657539327000, 0.000000000000000000, 18.54539866546729243 ) ) ;
#11713 = LINE ( 'NONE', #2158, #4197 ) ;
#11714 = LINE ( 'NONE', #3142, #2462 ) ;
#11715 = CARTESIAN_POINT ( 'NONE',  ( -30.80918829504999934, 27.97290950744599769, 64.35000000000000853 ) ) ;
#11716 = PLANE ( 'NONE',  #445 ) ;
#11717 =( NAMED_UNIT ( * ) PLANE_ANGLE_UNIT ( ) SI_UNIT ( $, .RADIAN. ) );
#11718 = VECTOR ( 'NONE', #7573, 1000.000000000000227 ) ;
#11719 = EDGE_LOOP ( 'NONE', ( #7985, #6280, #602, #12796 ) ) ;
#11720 = DIRECTION ( 'NONE',  ( 0.000000000000000000, 0.000000000000000000, -1.000000000000000000 ) ) ;
#11721 = EDGE_CURVE ( 'NONE', #9242, #6126, #7987, .T. ) ;
#11722 = VERTEX_POINT ( 'NONE', #5438 ) ;
#11723 = ORIENTED_EDGE ( 'NONE', *, *, #9793, .T. ) ;
#11724 = DIRECTION ( 'NONE',  ( 0.000000000000000000, 0.000000000000000000, 1.000000000000000000 ) ) ;
#11725 = CARTESIAN_POINT ( 'NONE',  ( -6.000000000000000888, -12.00000000000000178, 7.000000000000000000 ) ) ;
#11726 = LINE ( 'NONE', #8441, #4884 ) ;
#11727 = CARTESIAN_POINT ( 'NONE',  ( -35.05918829505000645, -6.027090492554000534, 64.85000000000000853 ) ) ;
#11728 = UNCERTAINTY_MEASURE_WITH_UNIT (LENGTH_MEASURE( 1.000000000000000082E-05 ), #6942, 'distance_accuracy_value', 'NONE');
#11729 = AXIS2_PLACEMENT_3D ( 'NONE', #12139, #1583, #13180 ) ;
#11730 = CARTESIAN_POINT ( 'NONE',  ( -18.05918829504999934, 10.97290950744599947, 57.35000000000000142 ) ) ;
#11731 = ORIENTED_EDGE ( 'NONE', *, *, #1546, .F. ) ;
#11732 = EDGE_CURVE ( 'NONE', #6593, #6180, #292, .T. ) ;
#11733 = ORIENTED_EDGE ( 'NONE', *, *, #221, .T. ) ;
#11734 = CARTESIAN_POINT ( 'NONE',  ( -18.05918829504999934, 10.97290950744599947, 62.14999999999999858 ) ) ;
#11735 = CARTESIAN_POINT ( 'NONE',  ( -4.599650328638321461, 8.500000000000000000, -5.878124499050807472 ) ) ;
#11736 = DIRECTION ( 'NONE',  ( -1.000000000000000000, 0.000000000000000000, 0.000000000000000000 ) ) ;
#11737 = ORIENTED_EDGE ( 'NONE', *, *, #3826, .T. ) ;
#11738 = CARTESIAN_POINT ( 'NONE',  ( 105.4499059006094654, 83.97306027416853169, 10.00000000000000000 ) ) ;
#11739 = CARTESIAN_POINT ( 'NONE',  ( -12.87735031270726083, -6.265087914666309210, 63.45000000000000284 ) ) ;
#11740 = CARTESIAN_POINT ( 'NONE',  ( -1.899121662050003101, 2.892876190445991202, 63.34900083300006202 ) ) ;
#11741 = AXIS2_PLACEMENT_3D ( 'NONE', #11976, #5541, #10032 ) ;
#11742 = FACE_BOUND ( 'NONE', #9682, .T. ) ;
#11743 = ORIENTED_EDGE ( 'NONE', *, *, #2226, .F. ) ;
#11744 = ORIENTED_EDGE ( 'NONE', *, *, #9531, .F. ) ;
#11745 = DIRECTION ( 'NONE',  ( 1.000000000000000000, 0.000000000000000000, 0.000000000000000000 ) ) ;
#11746 = ORIENTED_EDGE ( 'NONE', *, *, #4162, .T. ) ;
#11747 = EDGE_CURVE ( 'NONE', #7555, #2082, #2408, .T. ) ;
#11748 = ORIENTED_EDGE ( 'NONE', *, *, #10568, .T. ) ;
#11749 = ORIENTED_EDGE ( 'NONE', *, *, #1282, .F. ) ;
#11750 = AXIS2_PLACEMENT_3D ( 'NONE', #13607, #10275, #900 ) ;
#11751 = VERTEX_POINT ( 'NONE', #11738 ) ;
#11752 = CARTESIAN_POINT ( 'NONE',  ( 109.1537879975201406, 82.61803701715820125, 0.000000000000000000 ) ) ;
#11753 = DIRECTION ( 'NONE',  ( 0.000000000000000000, 0.000000000000000000, -1.000000000000000000 ) ) ;
#11754 = ORIENTED_EDGE ( 'NONE', *, *, #13648, .T. ) ;
#11755 = DIRECTION ( 'NONE',  ( -0.9576665234506835933, -0.2878798879079284001, 0.000000000000000000 ) ) ;
#11756 = DIRECTION ( 'NONE',  ( 1.000000000000000000, 0.000000000000000000, 0.000000000000000000 ) ) ;
#11757 = FACE_OUTER_BOUND ( 'NONE', #10830, .T. ) ;
#11758 = CARTESIAN_POINT ( 'NONE',  ( 43.38563590245419732, 110.7284214383315089, 20.00000000000000000 ) ) ;
#11759 = EDGE_CURVE ( 'NONE', #12630, #6080, #5507, .T. ) ;
#11760 = CARTESIAN_POINT ( 'NONE',  ( -35.72201093190194854, 10.97290950744599947, 5.250000000000000000 ) ) ;
#11761 =( BOUNDED_CURVE ( )  B_SPLINE_CURVE ( 3, ( #478, #7864, #10123, #12279 ),
 .UNSPECIFIED., .F., .F. ) 
 B_SPLINE_CURVE_WITH_KNOTS ( ( 4, 4 ),
 ( 4.712388980384689674, 6.283185307179586232 ),
 .UNSPECIFIED. ) 
 CURVE ( )  GEOMETRIC_REPRESENTATION_ITEM ( )  RATIONAL_B_SPLINE_CURVE ( ( 1.000000000000000000, 0.8047378541243649375, 0.8047378541243649375, 1.000000000000000000 ) ) 
 REPRESENTATION_ITEM ( '' )  );
#11762 = VERTEX_POINT ( 'NONE', #7392 ) ;
#11763 = EDGE_CURVE ( 'NONE', #5219, #10722, #13340, .T. ) ;
#11764 = DIRECTION ( 'NONE',  ( 0.000000000000000000, 0.000000000000000000, 1.000000000000000000 ) ) ;
#11765 = AXIS2_PLACEMENT_3D ( 'NONE', #11630, #7272, #5197 ) ;
#11766 = DIRECTION ( 'NONE',  ( 0.000000000000000000, 0.000000000000000000, 1.000000000000000000 ) ) ;
#11767 = VECTOR ( 'NONE', #6687, 1000.000000000000000 ) ;
#11768 = DIRECTION ( 'NONE',  ( 0.000000000000000000, 0.000000000000000000, 1.000000000000000000 ) ) ;
#11769 = CARTESIAN_POINT ( 'NONE',  ( 50.63563590245420443, 108.9054980190242503, 22.89644660940672694 ) ) ;
#11770 = STYLED_ITEM ( 'NONE', ( #12124 ), #9762 ) ;
#11771 = CARTESIAN_POINT ( 'NONE',  ( -20.82467356178127105, 30.19507513500936824, 54.34448619228547983 ) ) ;
#11772 = CARTESIAN_POINT ( 'NONE',  ( -7.241070169793059286, 29.81324547859994922, 17.25000000000000000 ) ) ;
#11773 = CARTESIAN_POINT ( 'NONE',  ( -2.819094421049990640, 3.352862570445993562, 61.63595870799996845 ) ) ;
#11774 = CARTESIAN_POINT ( 'NONE',  ( 142.6356359024541973, 87.03908161011133870, 19.25000000000000000 ) ) ;
#11775 = DIRECTION ( 'NONE',  ( 0.000000000000000000, 0.000000000000000000, 1.000000000000000000 ) ) ;
#11776 = EDGE_CURVE ( 'NONE', #7757, #68, #10769, .T. ) ;
#11777 = FACE_OUTER_BOUND ( 'NONE', #7895, .T. ) ;
#11778 = AXIS2_PLACEMENT_3D ( 'NONE', #11534, #780, #920 ) ;
#11779 = CIRCLE ( 'NONE', #5962, 1.999999999999994893 ) ;
#11780 = AXIS2_PLACEMENT_3D ( 'NONE', #4363, #12865, #3309 ) ;
#11781 = ORIENTED_EDGE ( 'NONE', *, *, #688, .F. ) ;
#11782 = EDGE_LOOP ( 'NONE', ( #1995, #3156 ) ) ;
#11783 = ORIENTED_EDGE ( 'NONE', *, *, #1151, .T. ) ;
#11784 = ORIENTED_EDGE ( 'NONE', *, *, #3229, .F. ) ;
#11785 = CARTESIAN_POINT ( 'NONE',  ( -1.059188295049996231, -6.027090492554000534, 7.250000000000000000 ) ) ;
#11786 = FACE_OUTER_BOUND ( 'NONE', #983, .T. ) ;
#11787 =( NAMED_UNIT ( * ) SI_UNIT ( $, .STERADIAN. ) SOLID_ANGLE_UNIT ( ) );
#11788 = ORIENTED_EDGE ( 'NONE', *, *, #8460, .T. ) ;
#11789 = AXIS2_PLACEMENT_3D ( 'NONE', #1610, #2682, #6839 ) ;
#11790 = AXIS2_PLACEMENT_3D ( 'NONE', #13030, #529, #6599 ) ;
#11791 = CARTESIAN_POINT ( 'NONE',  ( -35.05918829505000645, 27.97290950744599769, 58.85000000000000142 ) ) ;
#11792 = AXIS2_PLACEMENT_3D ( 'NONE', #1768, #2835, #12244 ) ;
#11793 = ADVANCED_FACE ( 'NONE', ( #9872 ), #3442, .T. ) ;
#11794 = CARTESIAN_POINT ( 'NONE',  ( -10.78334210919089919, 29.19143287883919768, 64.85000000000000853 ) ) ;
#11795 = FACE_OUTER_BOUND ( 'NONE', #8710, .T. ) ;
#11796 = AXIS2_PLACEMENT_3D ( 'NONE', #2723, #1647, #4030 ) ;
#11797 = ORIENTED_EDGE ( 'NONE', *, *, #221, .F. ) ;
#11798 = VECTOR ( 'NONE', #8807, 1000.000000000000000 ) ;
#11799 = DIRECTION ( 'NONE',  ( -0.000000000000000000, -0.000000000000000000, 1.000000000000000000 ) ) ;
#11800 = ORIENTED_EDGE ( 'NONE', *, *, #5164, .T. ) ;
#11801 = ORIENTED_EDGE ( 'NONE', *, *, #523, .T. ) ;
#11802 = VERTEX_POINT ( 'NONE', #5376 ) ;
#11803 = CARTESIAN_POINT ( 'NONE',  ( -11.70083760351054103, 35.47811937223634970, 17.25000000000000000 ) ) ;
#11804 = CYLINDRICAL_SURFACE ( 'NONE', #6478, 1.999999999999996669 ) ;
#11805 = CARTESIAN_POINT ( 'NONE',  ( 75.58559257550551536, 115.9888905337886769, 19.25000000000000000 ) ) ;
#11806 = EDGE_LOOP ( 'NONE', ( #1043, #733 ) ) ;
#11807 = ORIENTED_EDGE ( 'NONE', *, *, #9469, .F. ) ;
#11808 = DIRECTION ( 'NONE',  ( -0.7071067811865451302, 0.7071067811865500152, 0.000000000000000000 ) ) ;
#11809 = CARTESIAN_POINT ( 'NONE',  ( 123.1053058165644671, 129.5087515242213669, 19.25000000000000000 ) ) ;
#11810 = CARTESIAN_POINT ( 'NONE',  ( 42.63563590245419732, 85.03908161011133870, 0.7500000000000006661 ) ) ;
#11811 = CARTESIAN_POINT ( 'NONE',  ( -34.78181777225609750, 10.00028003023991907, 63.45000000000000284 ) ) ;
#11812 = AXIS2_PLACEMENT_3D ( 'NONE', #7905, #581, #6858 ) ;
#11813 = AXIS2_PLACEMENT_3D ( 'NONE', #9626, #8429, #3144 ) ;
#11814 = ADVANCED_FACE ( 'NONE', ( #8740 ), #136, .T. ) ;
#11815 = ADVANCED_FACE ( 'NONE', ( #11680 ), #4553, .F. ) ;
#11816 = ORIENTED_EDGE ( 'NONE', *, *, #1790, .F. ) ;
#11817 = ADVANCED_FACE ( 'NONE', ( #7667 ), #8805, .T. ) ;
#11818 = EDGE_LOOP ( 'NONE', ( #5206, #1280, #10352, #12123 ) ) ;
#11819 = ORIENTED_EDGE ( 'NONE', *, *, #5417, .T. ) ;
#11820 = CARTESIAN_POINT ( 'NONE',  ( -4.059188295049996675, -6.027090492554000534, 0.000000000000000000 ) ) ;
#11821 = ORIENTED_EDGE ( 'NONE', *, *, #8798, .F. ) ;
#11822 = VERTEX_POINT ( 'NONE', #211 ) ;
#11823 = ORIENTED_EDGE ( 'NONE', *, *, #155, .F. ) ;
#11824 = PRODUCT_DEFINITION_SHAPE ( 'NONE', 'NONE',  #13817 ) ;
#11825 = VECTOR ( 'NONE', #659, 1000.000000000000000 ) ;
#11826 = DIRECTION ( 'NONE',  ( -0.000000000000000000, -0.000000000000000000, -1.000000000000000000 ) ) ;
#11827 = CARTESIAN_POINT ( 'NONE',  ( 0.09777679598750591006, 23.36596564213564875, 7.250000000000000000 ) ) ;
#11828 = ORIENTED_EDGE ( 'NONE', *, *, #4395, .F. ) ;
#11829 = FACE_OUTER_BOUND ( 'NONE', #11278, .T. ) ;
#11830 = CARTESIAN_POINT ( 'NONE',  ( 0.000000000000000000, 4.500000000000000000, 0.000000000000000000 ) ) ;
#11831 = CARTESIAN_POINT ( 'NONE',  ( 50.38563590245420443, 108.9054980190242503, 22.75000000000000000 ) ) ;
#11832 = CYLINDRICAL_SURFACE ( 'NONE', #6723, 4.000000000000000888 ) ;
#11833 = CARTESIAN_POINT ( 'NONE',  ( 1.097360187335109982, -3.327306731351814761, 68.85549045786049760 ) ) ;
#11834 = APPLICATION_PROTOCOL_DEFINITION ( 'draft international standard', 'automotive_design', 1998, #8137 ) ;
#11835 = EDGE_CURVE ( 'NONE', #10693, #1263, #2676, .T. ) ;
#11836 = VECTOR ( 'NONE', #1871, 1000.000000000000227 ) ;
#11837 = VECTOR ( 'NONE', #5107, 1000.000000000000000 ) ;
#11838 = VECTOR ( 'NONE', #8187, 1000.000000000000114 ) ;
#11839 = VECTOR ( 'NONE', #1661, 1000.000000000000114 ) ;
#11840 = ORIENTED_EDGE ( 'NONE', *, *, #5959, .F. ) ;
#11841 = EDGE_LOOP ( 'NONE', ( #9664, #1740, #1477, #1434, #185, #3946 ) ) ;
#11842 = EDGE_CURVE ( 'NONE', #7821, #13545, #5583, .T. ) ;
#11843 = LINE ( 'NONE', #4374, #8594 ) ;
#11844 = CARTESIAN_POINT ( 'NONE',  ( 84.99521369064696330, 82.14063840035363739, 10.00000000000000000 ) ) ;
#11845 = DIRECTION ( 'NONE',  ( -0.6615960714621568206, 0.7498604124941127269, 0.000000000000000000 ) ) ;
#11846 = CARTESIAN_POINT ( 'NONE',  ( -20.35918349919666781, 30.24616810948638701, 53.87192440031903118 ) ) ;
#11847 = VECTOR ( 'NONE', #8252, 1000.000000000000000 ) ;
#11848 = SHAPE_REPRESENTATION ( 'BR-Y-110', ( #8232, #9569, #7535, #5770, #11796, #6445, #1545, #9356, #875, #3337, #10251, #11138, #3118 ), #6659 ) ;
#11849 = CIRCLE ( 'NONE', #11619, 6.450000000000019718 ) ;
#11850 = CARTESIAN_POINT ( 'NONE',  ( -18.05918829504999934, 10.97290950744599947, 62.85000000000000142 ) ) ;
#11851 = DIRECTION ( 'NONE',  ( -1.000000000000000000, 0.000000000000000000, 0.000000000000000000 ) ) ;
#11852 = CIRCLE ( 'NONE', #6275, 16.72262947720610171 ) ;
#11853 = FACE_OUTER_BOUND ( 'NONE', #5329, .T. ) ;
#11854 = FACE_OUTER_BOUND ( 'NONE', #5725, .T. ) ;
#11855 = CARTESIAN_POINT ( 'NONE',  ( -1.059188295049996231, 10.97290950744599947, 64.35000000000000853 ) ) ;
#11856 = DIRECTION ( 'NONE',  ( 1.000000000000000000, 0.000000000000000000, 0.000000000000000000 ) ) ;
#11857 = EDGE_CURVE ( 'NONE', #10813, #8521, #4349, .T. ) ;
#11858 = EDGE_CURVE ( 'NONE', #12302, #5782, #8527, .T. ) ;
#11859 = AXIS2_PLACEMENT_3D ( 'NONE', #8873, #12020, #3708 ) ;
#11860 = CIRCLE ( 'NONE', #8960, 8.250000000000001776 ) ;
#11861 = VECTOR ( 'NONE', #8134, 1000.000000000000000 ) ;
#11862 = ORIENTED_EDGE ( 'NONE', *, *, #9969, .T. ) ;
#11863 = ADVANCED_FACE ( 'NONE', ( #6364 ), #5318, .T. ) ;
#11864 = VERTEX_POINT ( 'NONE', #7 ) ;
#11865 = DIRECTION ( 'NONE',  ( 0.9496839325805416232, 0.3132098788326400096, 0.000000000000000000 ) ) ;
#11866 = EDGE_LOOP ( 'NONE', ( #6005, #13558, #3549, #7456, #10522, #6102 ) ) ;
#11867 = EDGE_LOOP ( 'NONE', ( #11293, #12378, #7160, #12592 ) ) ;
#11868 = VERTEX_POINT ( 'NONE', #9654 ) ;
#11869 = ORIENTED_EDGE ( 'NONE', *, *, #1488, .F. ) ;
#11870 = CARTESIAN_POINT ( 'NONE',  ( -10.44110272205000101, 10.97290950744599947, 61.65955166399999854 ) ) ;
#11871 = DIRECTION ( 'NONE',  ( -0.000000000000000000, -0.000000000000000000, 1.000000000000000000 ) ) ;
#11872 = DIRECTION ( 'NONE',  ( 0.000000000000000000, 0.000000000000000000, -1.000000000000000000 ) ) ;
#11873 = DIRECTION ( 'NONE',  ( 0.000000000000000000, 0.000000000000000000, -1.000000000000000000 ) ) ;
#11874 = PLANE ( 'NONE',  #3598 ) ;
#11875 = AXIS2_PLACEMENT_3D ( 'NONE', #7584, #11872, #9768 ) ;
#11876 = FACE_OUTER_BOUND ( 'NONE', #4558, .T. ) ;
#11877 = LINE ( 'NONE', #6620, #3983 ) ;
#11878 = EDGE_CURVE ( 'NONE', #209, #5173, #73, .T. ) ;
#11879 = VERTEX_POINT ( 'NONE', #2267 ) ;
#11880 = EDGE_CURVE ( 'NONE', #997, #3420, #6507, .T. ) ;
#11881 = CARTESIAN_POINT ( 'NONE',  ( -15.78544589689968802, 30.24873049213536191, 53.85022182113912947 ) ) ;
#11882 = DIRECTION ( 'NONE',  ( 1.000000000000000000, 0.000000000000000000, 0.000000000000000000 ) ) ;
#11883 = DIRECTION ( 'NONE',  ( 1.000000000000000000, 0.000000000000000000, 0.000000000000000000 ) ) ;
#11884 = ORIENTED_EDGE ( 'NONE', *, *, #11335, .F. ) ;
#11885 = ORIENTED_EDGE ( 'NONE', *, *, #5106, .T. ) ;
#11886 = CARTESIAN_POINT ( 'NONE',  ( 8.157609394192110841, 24.73469418910620021, 17.25000000000000000 ) ) ;
#11887 = PLANE ( 'NONE',  #6903 ) ;
#11888 = DIRECTION ( 'NONE',  ( -0.000000000000000000, -0.000000000000000000, -1.000000000000000000 ) ) ;
#11889 = STYLED_ITEM ( 'NONE', ( #4728 ), #5212 ) ;
#11890 = ORIENTED_EDGE ( 'NONE', *, *, #8319, .T. ) ;
#11891 = VERTEX_POINT ( 'NONE', #5790 ) ;
#11892 = ORIENTED_EDGE ( 'NONE', *, *, #4950, .F. ) ;
#11893 = DIRECTION ( 'NONE',  ( 0.7071067811865524577, 0.7071067811865425767, -0.000000000000000000 ) ) ;
#11894 = ORIENTED_EDGE ( 'NONE', *, *, #350, .T. ) ;
#11895 = ORIENTED_EDGE ( 'NONE', *, *, #4011, .F. ) ;
#11896 = ORIENTED_EDGE ( 'NONE', *, *, #4590, .T. ) ;
#11897 = AXIS2_PLACEMENT_3D ( 'NONE', #9814, #2355, #236 ) ;
#11898 = ORIENTED_EDGE ( 'NONE', *, *, #8687, .T. ) ;
#11899 = DIRECTION ( 'NONE',  ( -0.000000000000000000, 1.000000000000000000, -0.000000000000000000 ) ) ;
#11900 = EDGE_CURVE ( 'NONE', #8158, #7243, #12091, .T. ) ;
#11901 = CARTESIAN_POINT ( 'NONE',  ( -18.05918829504999934, 10.97290950744599947, 57.35000000000000142 ) ) ;
#11902 = VERTEX_POINT ( 'NONE', #11113 ) ;
#11903 = CARTESIAN_POINT ( 'NONE',  ( -3.999999999999997335, 2.000000000000000000, 0.000000000000000000 ) ) ;
#11904 = DIRECTION ( 'NONE',  ( 1.000000000000000000, 0.000000000000000000, 0.000000000000000000 ) ) ;
#11905 = LINE ( 'NONE', #12311, #8872 ) ;
#11906 = DIRECTION ( 'NONE',  ( -1.000000000000000000, 0.000000000000000000, 0.000000000000000000 ) ) ;
#11907 = CARTESIAN_POINT ( 'NONE',  ( -35.05918829505000645, -6.027090492554000534, 0.000000000000000000 ) ) ;
#11908 = CONTEXT_DEPENDENT_SHAPE_REPRESENTATION ( #10466, #10710 ) ;
#11909 = CIRCLE ( 'NONE', #11024, 2.800000000000000266 ) ;
#11910 = EDGE_LOOP ( 'NONE', ( #12324, #4387, #3173, #5524 ) ) ;
#11911 = ORIENTED_EDGE ( 'NONE', *, *, #6291, .T. ) ;
#11912 = ORIENTED_EDGE ( 'NONE', *, *, #7920, .F. ) ;
#11913 = DIRECTION ( 'NONE',  ( -8.673617379884027583E-16, -1.000000000000000000, 0.000000000000000000 ) ) ;
#11914 = FACE_BOUND ( 'NONE', #4416, .T. ) ;
#11915 = ORIENTED_EDGE ( 'NONE', *, *, #10970, .F. ) ;
#11916 = FACE_OUTER_BOUND ( 'NONE', #1941, .T. ) ;
#11917 = ADVANCED_FACE ( 'NONE', ( #11180 ), #5098, .F. ) ;
#11918 = CARTESIAN_POINT ( 'NONE',  ( -4.059188295049996675, -6.027090492554000534, 10.00000000000000000 ) ) ;
#11919 = CARTESIAN_POINT ( 'NONE',  ( -18.82359282014710544, 30.34769730472570970, 53.07963013742637060 ) ) ;
#11920 = CARTESIAN_POINT ( 'NONE',  ( -17.23821357112329977, 5.029341513162310484, 68.84999999999999432 ) ) ;
#11921 = CARTESIAN_POINT ( 'NONE',  ( -15.41280400920135030, 7.973467857469549891, 30.59999999999999787 ) ) ;
#11922 = DIRECTION ( 'NONE',  ( 0.000000000000000000, 0.000000000000000000, 1.000000000000000000 ) ) ;
#11923 = CARTESIAN_POINT ( 'NONE',  ( 0.000000000000000000, 4.500000000000000000, 0.000000000000000000 ) ) ;
#11924 = ADVANCED_FACE ( 'NONE', ( #8029 ), #2549, .T. ) ;
#11925 = LINE ( 'NONE', #13172, #1322 ) ;
#11926 = ORIENTED_EDGE ( 'NONE', *, *, #13685, .T. ) ;
#11927 =( BOUNDED_CURVE ( )  B_SPLINE_CURVE ( 3, ( #5032, #8524, #10487, #9447 ),
 .UNSPECIFIED., .F., .F. ) 
 B_SPLINE_CURVE_WITH_KNOTS ( ( 4, 4 ),
 ( 1.570796326794896558, 3.141592653589793116 ),
 .UNSPECIFIED. ) 
 CURVE ( )  GEOMETRIC_REPRESENTATION_ITEM ( )  RATIONAL_B_SPLINE_CURVE ( ( 1.000000000000000000, 0.8047378541243649375, 0.8047378541243649375, 1.000000000000000000 ) ) 
 REPRESENTATION_ITEM ( '' )  );
#11928 = FACE_BOUND ( 'NONE', #1040, .T. ) ;
#11929 = VERTEX_POINT ( 'NONE', #4820 ) ;
#11930 = VERTEX_POINT ( 'NONE', #6908 ) ;
#11931 = CYLINDRICAL_SURFACE ( 'NONE', #9160, 1.999999999999986233 ) ;
#11933 = EDGE_CURVE ( 'NONE', #9462, #5579, #500, .T. ) ;
#11932 = ORIENTED_EDGE ( 'NONE', *, *, #13612, .F. ) ;
#11934 = DIRECTION ( 'NONE',  ( 1.000000000000000000, 0.000000000000000000, -0.000000000000000000 ) ) ;
#11935 = CARTESIAN_POINT ( 'NONE',  ( 185.2712718049083946, 104.1554980190242361, 23.00000000000000000 ) ) ;
#11936 = CARTESIAN_POINT ( 'NONE',  ( 9.640422211807132769, 16.89844320975774750, 0.000000000000000000 ) ) ;
#11937 = VERTEX_POINT ( 'NONE', #10075 ) ;
#11938 = DIRECTION ( 'NONE',  ( -0.000000000000000000, 1.000000000000000000, -0.000000000000000000 ) ) ;
#11939 = CYLINDRICAL_SURFACE ( 'NONE', #854, 3.000000000000002665 ) ;
#11940 = LINE ( 'NONE', #2325, #5146 ) ;
#11941 = CARTESIAN_POINT ( 'NONE',  ( 18.45469220996244886, 1.832421873814834123, 0.000000000000000000 ) ) ;
#11942 = LINE ( 'NONE', #7728, #2435 ) ;
#11943 = EDGE_CURVE ( 'NONE', #10781, #12773, #1402, .T. ) ;
#11944 = CLOSED_SHELL ( 'NONE', ( #7529, #34, #5687, #4014, #3749, #11523 ) ) ;
#11945 = ORIENTED_EDGE ( 'NONE', *, *, #2330, .F. ) ;
#11946 = CARTESIAN_POINT ( 'NONE',  ( -17.10968755856460177, 30.34086823225404217, 53.12849656952644750 ) ) ;
#11948 = ORIENTED_EDGE ( 'NONE', *, *, #12459, .F. ) ;
#11947 = EDGE_CURVE ( 'NONE', #9990, #11959, #6661, .T. ) ;
#11949 = CARTESIAN_POINT ( 'NONE',  ( 7.500000000000000000, -0.5000000000000017764, -65.00000000000000000 ) ) ;
#11950 = FILL_AREA_STYLE ('',( #4404 ) ) ;
#11951 = EDGE_LOOP ( 'NONE', ( #2540, #12925, #1658, #5204, #5384, #6444, #11807, #12300, #1999, #5871, #2848, #1077, #4686, #11292, #3464, #366, #10394, #6394, #2239, #317 ) ) ;
#11952 = DIRECTION ( 'NONE',  ( 1.000000000000000000, 0.000000000000000000, 0.000000000000000000 ) ) ;
#11953 = CARTESIAN_POINT ( 'NONE',  ( -18.05918829504999934, 10.97290950744599947, 57.35000000000000142 ) ) ;
#11954 = EDGE_CURVE ( 'NONE', #13684, #5561, #9156, .T. ) ;
#11955 = FACE_OUTER_BOUND ( 'NONE', #4645, .T. ) ;
#11956 = CIRCLE ( 'NONE', #13513, 1.999999999999991340 ) ;
#11957 = ORIENTED_EDGE ( 'NONE', *, *, #1865, .T. ) ;
#11958 = EDGE_LOOP ( 'NONE', ( #8463, #1277, #4549, #13509 ) ) ;
#11959 = VERTEX_POINT ( 'NONE', #3709 ) ;
#11960 = DIRECTION ( 'NONE',  ( 1.000000000000000000, 0.000000000000000000, 0.000000000000000000 ) ) ;
#11961 = ORIENTED_EDGE ( 'NONE', *, *, #6171, .F. ) ;
#11962 = ORIENTED_EDGE ( 'NONE', *, *, #3076, .T. ) ;
#11963 = VERTEX_POINT ( 'NONE', #426 ) ;
#11964 = DIRECTION ( 'NONE',  ( 1.000000000000000000, 0.000000000000000000, 0.000000000000000000 ) ) ;
#11965 = CARTESIAN_POINT ( 'NONE',  ( -18.05918829504999934, 10.97290950744599947, 62.14999999999999858 ) ) ;
#11966 = ORIENTED_EDGE ( 'NONE', *, *, #9469, .T. ) ;
#11967 = VECTOR ( 'NONE', #11015, 1000.000000000000000 ) ;
#11968 = DIRECTION ( 'NONE',  ( 0.000000000000000000, 1.000000000000000000, 0.000000000000000000 ) ) ;
#11969 = CARTESIAN_POINT ( 'NONE',  ( -16.65773704950522927, 26.91141943044650375, 56.81390271690813876 ) ) ;
#11970 = CARTESIAN_POINT ( 'NONE',  ( 98.27605811426136029, 115.9375248198690826, 20.00000000000000000 ) ) ;
#11971 = DIRECTION ( 'NONE',  ( 0.000000000000000000, 0.000000000000000000, -1.000000000000000000 ) ) ;
#11972 = CYLINDRICAL_SURFACE ( 'NONE', #9590, 2.000000000000001776 ) ;
#11973 = EDGE_CURVE ( 'NONE', #13550, #5000, #3324, .T. ) ;
#11974 = CIRCLE ( 'NONE', #2629, 2.999999999999998224 ) ;
#11975 = VERTEX_POINT ( 'NONE', #9073 ) ;
#11976 = CARTESIAN_POINT ( 'NONE',  ( 42.63563590245419732, 85.03908161011133870, 20.00000000000000000 ) ) ;
#11977 = DIRECTION ( 'NONE',  ( -1.000000000000000000, 0.000000000000000000, 0.000000000000000000 ) ) ;
#11978 = DIRECTION ( 'NONE',  ( 0.000000000000000000, 0.000000000000000000, -1.000000000000000000 ) ) ;
#11979 = DIRECTION ( 'NONE',  ( 0.000000000000000000, 1.000000000000000000, 0.000000000000000000 ) ) ;
#11980 = CARTESIAN_POINT ( 'NONE',  ( -19.10270367411500203, 30.33713881009503410, 53.15513206184487416 ) ) ;
#11981 = LINE ( 'NONE', #2442, #6308 ) ;
#11982 = ORIENTED_EDGE ( 'NONE', *, *, #7081, .T. ) ;
#11983 = VECTOR ( 'NONE', #4312, 999.9999999999998863 ) ;
#11984 = CARTESIAN_POINT ( 'NONE',  ( -18.05918829504999934, 10.97290950744599947, 67.84999999999999432 ) ) ;
#11985 = ADVANCED_FACE ( 'NONE', ( #6777 ), #12026, .T. ) ;
#11986 = DIRECTION ( 'NONE',  ( -1.000000000000000000, 0.000000000000000000, 0.000000000000000000 ) ) ;
#11987 = CARTESIAN_POINT ( 'NONE',  ( -35.05918829505000645, 27.97290950744599769, 5.250000000000000000 ) ) ;
#11988 = CIRCLE ( 'NONE', #4408, 4.750000000000000888 ) ;
#11989 = CARTESIAN_POINT ( 'NONE',  ( -35.05918829505000645, -6.027090492554000534, 64.85000000000000853 ) ) ;
#11990 = EDGE_CURVE ( 'NONE', #6295, #3941, #5651, .T. ) ;
#11991 = ADVANCED_FACE ( 'NONE', ( #5920 ), #11256, .T. ) ;
#11992 = ADVANCED_FACE ( 'NONE', ( #7888 ), #2001, .T. ) ;
#11993 = AXIS2_PLACEMENT_3D ( 'NONE', #2010, #4158, #7543 ) ;
#11994 =( GEOMETRIC_REPRESENTATION_CONTEXT ( 3 ) GLOBAL_UNCERTAINTY_ASSIGNED_CONTEXT ( ( #11728 ) ) GLOBAL_UNIT_ASSIGNED_CONTEXT ( ( #6942, #11217, #3470 ) ) REPRESENTATION_CONTEXT ( 'NONE', 'WORKASPACE' ) );
#11995 = CARTESIAN_POINT ( 'NONE',  ( -18.45469220996244886, -1.832421873814834123, 7.000000000000000000 ) ) ;
#11996 = DIRECTION ( 'NONE',  ( 1.000000000000000000, 0.000000000000000000, 0.000000000000000000 ) ) ;
#11997 = ORIENTED_EDGE ( 'NONE', *, *, #4399, .T. ) ;
#11998 = PLANE ( 'NONE',  #10494 ) ;
#11999 = CARTESIAN_POINT ( 'NONE',  ( -11.74835982676941981, -4.028726038184999858, 62.14999999999999858 ) ) ;
#12000 = DIRECTION ( 'NONE',  ( 0.000000000000000000, 1.000000000000000000, 0.000000000000000000 ) ) ;
#12001 = DIRECTION ( 'NONE',  ( 1.577021341797097560E-16, -1.000000000000000000, 0.000000000000000000 ) ) ;
#12002 = EDGE_CURVE ( 'NONE', #10219, #5663, #5759, .T. ) ;
#12003 = FACE_BOUND ( 'NONE', #5808, .T. ) ;
#12004 = DIRECTION ( 'NONE',  ( -0.000000000000000000, 1.000000000000000000, -0.000000000000000000 ) ) ;
#12005 = CARTESIAN_POINT ( 'NONE',  ( 134.6356359024541973, 94.90549801902425031, 20.00000000000000000 ) ) ;
#12006 = DIRECTION ( 'NONE',  ( 0.000000000000000000, 0.000000000000000000, 1.000000000000000000 ) ) ;
#12007 = CIRCLE ( 'NONE', #9552, 6.419999999999999929 ) ;
#12008 = AXIS2_PLACEMENT_3D ( 'NONE', #12667, #7336, #11296 ) ;
#12009 = AXIS2_PLACEMENT_3D ( 'NONE', #12778, #5428, #4335 ) ;
#12010 = AXIS2_PLACEMENT_3D ( 'NONE', #2627, #10853, #2562 ) ;
#12011 = ADVANCED_FACE ( 'NONE', ( #1468, #5717 ), #4695, .F. ) ;
#12012 = EDGE_LOOP ( 'NONE', ( #5628, #9315, #5757, #6222 ) ) ;
#12013 = DIRECTION ( 'NONE',  ( -1.000000000000000000, 0.000000000000000000, 0.000000000000000000 ) ) ;
#12014 = AXIS2_PLACEMENT_3D ( 'NONE', #9450, #13754, #8391 ) ;
#12015 = VECTOR ( 'NONE', #12371, 1000.000000000000114 ) ;
#12016 = ORIENTED_EDGE ( 'NONE', *, *, #3243, .T. ) ;
#12017 = CARTESIAN_POINT ( 'NONE',  ( -18.05918829504999934, 10.97290950744599947, 63.14999999999999858 ) ) ;
#12018 = AXIS2_PLACEMENT_3D ( 'NONE', #9057, #7024, #6961 ) ;
#12019 = PLANE ( 'NONE',  #12283 ) ;
#12020 = DIRECTION ( 'NONE',  ( 1.000000000000000000, 0.000000000000000000, -0.000000000000000000 ) ) ;
#12021 = EDGE_LOOP ( 'NONE', ( #5915, #2524, #12954, #9429 ) ) ;
#12022 = CARTESIAN_POINT ( 'NONE',  ( -16.40519811639460102, 9.098258476210720147, 67.84999999999999432 ) ) ;
#12023 = CARTESIAN_POINT ( 'NONE',  ( 4.000000000000001776, 2.000000000000000000, -65.00000000000000000 ) ) ;
#12024 = DIRECTION ( 'NONE',  ( -0.000000000000000000, -0.000000000000000000, 1.000000000000000000 ) ) ;
#12025 = PRODUCT_DEFINITION_FORMATION_WITH_SPECIFIED_SOURCE ( 'ANY', '', #162, .NOT_KNOWN. ) ;
#12026 = CONICAL_SURFACE ( 'NONE', #9348, 16.75000000000000355, 0.7853981633974447263 ) ;
#12027 = AXIS2_PLACEMENT_3D ( 'NONE', #9960, #7852, #2578 ) ;
#12028 = EDGE_CURVE ( 'NONE', #5017, #9550, #8000, .T. ) ;
#12029 = AXIS2_PLACEMENT_3D ( 'NONE', #6540, #8699, #1156 ) ;
#12030 = EDGE_CURVE ( 'NONE', #2858, #1798, #3567, .T. ) ;
#12031 = CARTESIAN_POINT ( 'NONE',  ( 142.3249757306743675, 110.9104019536709274, 19.99999999999999289 ) ) ;
#12032 = EDGE_LOOP ( 'NONE', ( #8981, #11869, #1982, #218 ) ) ;
#12033 = VERTEX_POINT ( 'NONE', #10403 ) ;
#12034 = EDGE_CURVE ( 'NONE', #10707, #10997, #9901, .T. ) ;
#12035 = ORIENTED_EDGE ( 'NONE', *, *, #5287, .T. ) ;
#12036 = CARTESIAN_POINT ( 'NONE',  ( 142.6356359024541973, 87.03908161011133870, 20.00000000000000000 ) ) ;
#12037 = CARTESIAN_POINT ( 'NONE',  ( -41.50918829505000218, -6.027090492554000534, 17.25000000000000000 ) ) ;
#12038 = ORIENTED_EDGE ( 'NONE', *, *, #11947, .T. ) ;
#12039 = DIRECTION ( 'NONE',  ( 1.000000000000000000, 0.000000000000000000, 0.000000000000000000 ) ) ;
#12040 = VECTOR ( 'NONE', #11207, 1000.000000000000000 ) ;
#12041 = LINE ( 'NONE', #5733, #7183 ) ;
#12042 = VECTOR ( 'NONE', #11653, 1000.000000000000000 ) ;
#12043 = DIRECTION ( 'NONE',  ( 1.000000000000000000, 0.000000000000000000, 0.000000000000000000 ) ) ;
#12044 = CARTESIAN_POINT ( 'NONE',  ( 27.50000000000001066, 9.000000000000000000, -30.00000000000000355 ) ) ;
#12045 = AXIS2_PLACEMENT_3D ( 'NONE', #6887, #11092, #7713 ) ;
#12046 = CIRCLE ( 'NONE', #6473, 16.95000000000000284 ) ;
#12047 = ORIENTED_EDGE ( 'NONE', *, *, #5244, .T. ) ;
#12048 = EDGE_CURVE ( 'NONE', #8944, #9587, #12901, .T. ) ;
#12049 = CARTESIAN_POINT ( 'NONE',  ( -18.05918829504999934, 10.97290950744599947, 62.14999999999999858 ) ) ;
#12050 = ORIENTED_EDGE ( 'NONE', *, *, #3970, .F. ) ;
#12051 = CARTESIAN_POINT ( 'NONE',  ( -24.20502162805000168, 10.97290950744599947, 60.60999999999999943 ) ) ;
#12052 = CARTESIAN_POINT ( 'NONE',  ( -20.82417809436781297, 30.19514031291545919, 60.35623975441919242 ) ) ;
#12053 = DIRECTION ( 'NONE',  ( 1.000000000000000000, 0.000000000000000000, 0.000000000000000000 ) ) ;
#12054 = FACE_OUTER_BOUND ( 'NONE', #11601, .T. ) ;
#12055 = DIRECTION ( 'NONE',  ( 0.000000000000000000, 0.000000000000000000, 1.000000000000000000 ) ) ;
#12056 = DIRECTION ( 'NONE',  ( 0.000000000000000000, 0.000000000000000000, 1.000000000000000000 ) ) ;
#12057 = CARTESIAN_POINT ( 'NONE',  ( -5.631644894983189431, 10.97290950744599947, 64.85000000000000853 ) ) ;
#12058 = AXIS2_PLACEMENT_3D ( 'NONE', #12278, #11365, #10258 ) ;
#12059 = AXIS2_PLACEMENT_3D ( 'NONE', #5503, #7811, #2186 ) ;
#12060 = AXIS2_PLACEMENT_3D ( 'NONE', #3445, #12024, #2478 ) ;
#12061 = AXIS2_PLACEMENT_3D ( 'NONE', #9059, #408, #13318 ) ;
#12062 = CARTESIAN_POINT ( 'NONE',  ( -16.08092853089235774, 4.500000000000000000, 9.237812082545083570 ) ) ;
#12063 = AXIS2_PLACEMENT_3D ( 'NONE', #1385, #8510, #1098 ) ;
#12064 = CARTESIAN_POINT ( 'NONE',  ( 0.000000000000000000, 0.000000000000000000, 0.000000000000000000 ) ) ;
#12065 = AXIS2_PLACEMENT_3D ( 'NONE', #11987, #13031, #4524 ) ;
#12066 = VERTEX_POINT ( 'NONE', #7240 ) ;
#12067 = ORIENTED_EDGE ( 'NONE', *, *, #9916, .T. ) ;
#12068 = PLANE ( 'NONE',  #13387 ) ;
#12069 = CARTESIAN_POINT ( 'NONE',  ( -3.499999999999998224, 2.499999999999999556, 0.000000000000000000 ) ) ;
#12070 = DIRECTION ( 'NONE',  ( 0.000000000000000000, -1.000000000000000000, 0.000000000000000000 ) ) ;
#12071 = CARTESIAN_POINT ( 'NONE',  ( -18.05918829504999934, 14.81548537210212046, 7.250000000000000000 ) ) ;
#12072 = CARTESIAN_POINT ( 'NONE',  ( 140.6356359024541973, 90.15549801902423610, 23.00000000000000000 ) ) ;
#12073 = EDGE_CURVE ( 'NONE', #2221, #1954, #12431, .T. ) ;
#12074 = CARTESIAN_POINT ( 'NONE',  ( 140.6356359024541973, 113.0390816101113387, 19.25000000000000000 ) ) ;
#12075 = DIRECTION ( 'NONE',  ( 1.000000000000000000, 0.000000000000000000, 0.000000000000000000 ) ) ;
#12076 = EDGE_CURVE ( 'NONE', #12394, #5520, #8991, .T. ) ;
#12077 = FACE_OUTER_BOUND ( 'NONE', #12534, .T. ) ;
#12078 = CARTESIAN_POINT ( 'NONE',  ( -35.05918829505000645, 27.97290950744599769, 83.57661607529820458 ) ) ;
#12079 = DIRECTION ( 'NONE',  ( 0.000000000000000000, 0.000000000000000000, 1.000000000000000000 ) ) ;
#12080 = VECTOR ( 'NONE', #5859, 1000.000000000000000 ) ;
#12081 = AXIS2_PLACEMENT_3D ( 'NONE', #9208, #6259, #12412 ) ;
#12082 = CIRCLE ( 'NONE', #1828, 17.00000000000000355 ) ;
#12083 = ORIENTED_EDGE ( 'NONE', *, *, #13379, .T. ) ;
#12084 = ORIENTED_EDGE ( 'NONE', *, *, #10678, .F. ) ;
#12085 = PLANE ( 'NONE',  #7687 ) ;
#12086 = EDGE_LOOP ( 'NONE', ( #4220, #9887 ) ) ;
#12087 = DIRECTION ( 'NONE',  ( 0.000000000000000000, 0.000000000000000000, 1.000000000000000000 ) ) ;
#12088 = MECHANICAL_DESIGN_GEOMETRIC_PRESENTATION_REPRESENTATION (  '', ( #5833 ), #4072 ) ;
#12089 = FACE_OUTER_BOUND ( 'NONE', #2813, .T. ) ;
#12090 = DIRECTION ( 'NONE',  ( 1.000000000000000000, 0.000000000000000000, 0.000000000000000000 ) ) ;
#12091 = LINE ( 'NONE', #12022, #195 ) ;
#12092 = EDGE_CURVE ( 'NONE', #12928, #2900, #860, .T. ) ;
#12093 = EDGE_CURVE ( 'NONE', #7102, #6443, #5226, .T. ) ;
#12094 = CARTESIAN_POINT ( 'NONE',  ( -1.461186629049982422, 19.27191034044602347, 63.13003331700004850 ) ) ;
#12095 = LINE ( 'NONE', #4556, #10033 ) ;
#12096 = PRODUCT_RELATED_PRODUCT_CATEGORY ( 'part', '', ( #10774 ) ) ;
#12097 = AXIS2_PLACEMENT_3D ( 'NONE', #8698, #11019, #2509 ) ;
#12098 = EDGE_CURVE ( 'NONE', #3533, #1109, #691, .T. ) ;
#12099 = ORIENTED_EDGE ( 'NONE', *, *, #13177, .F. ) ;
#12100 = VERTEX_POINT ( 'NONE', #7308 ) ;
#12101 = EDGE_LOOP ( 'NONE', ( #3417, #1258, #11966, #9022 ) ) ;
#12102 = ORIENTED_EDGE ( 'NONE', *, *, #5707, .T. ) ;
#12103 = CARTESIAN_POINT ( 'NONE',  ( 16.04064420431708982, 0.000000000000000000, 9.307586582922137808 ) ) ;
#12104 = ORIENTED_EDGE ( 'NONE', *, *, #12977, .T. ) ;
#12105 = ORIENTED_EDGE ( 'NONE', *, *, #4569, .T. ) ;
#12106 = EDGE_LOOP ( 'NONE', ( #7055, #13630, #8828, #4866 ) ) ;
#12107 = DIRECTION ( 'NONE',  ( 1.000000000000000000, 0.000000000000000000, 0.000000000000000000 ) ) ;
#12108 = PRESENTATION_LAYER_ASSIGNMENT (  '', '', ( #9212 ) ) ;
#12109 = DIRECTION ( 'NONE',  ( 0.000000000000000000, 0.000000000000000000, 1.000000000000000000 ) ) ;
#12110 = EDGE_CURVE ( 'NONE', #7324, #4724, #6870, .T. ) ;
#12111 = ORIENTED_EDGE ( 'NONE', *, *, #12153, .F. ) ;
#12112 = DIRECTION ( 'NONE',  ( 0.000000000000000000, 0.000000000000000000, 1.000000000000000000 ) ) ;
#12113 = AXIS2_PLACEMENT_3D ( 'NONE', #4789, #6031, #10308 ) ;
#12114 = CARTESIAN_POINT ( 'NONE',  ( -10.38347696868452097, 26.08535324214045303, 61.65000000000000568 ) ) ;
#12115 = CARTESIAN_POINT ( 'NONE',  ( 4.000000000000001776, 2.000000000000000000, 0.000000000000000000 ) ) ;
#12116 = FACE_OUTER_BOUND ( 'NONE', #10121, .T. ) ;
#12117 = EDGE_CURVE ( 'NONE', #1633, #6090, #8311, .T. ) ;
#12118 = EDGE_LOOP ( 'NONE', ( #1054, #9520, #4906, #13221 ) ) ;
#12119 = AXIS2_PLACEMENT_3D ( 'NONE', #6856, #3727, #5038 ) ;
#12120 = ORIENTED_EDGE ( 'NONE', *, *, #11842, .F. ) ;
#12121 = ORIENTED_EDGE ( 'NONE', *, *, #11377, .T. ) ;
#12122 = PLANE ( 'NONE',  #11741 ) ;
#12123 = ORIENTED_EDGE ( 'NONE', *, *, #14, .T. ) ;
#12124 = PRESENTATION_STYLE_ASSIGNMENT (( #9956 ) ) ;
#12125 = EDGE_CURVE ( 'NONE', #11930, #5595, #10447, .T. ) ;
#12126 = CARTESIAN_POINT ( 'NONE',  ( -21.58198509594925341, 30.09164131411911924, 59.05576624416044496 ) ) ;
#12127 = EDGE_LOOP ( 'NONE', ( #10362, #2318 ) ) ;
#12128 = CARTESIAN_POINT ( 'NONE',  ( 109.6856792294029219, 115.9888905337886769, 0.7500000000000006661 ) ) ;
#12129 = DIRECTION ( 'NONE',  ( 0.000000000000000000, 0.000000000000000000, 1.000000000000000000 ) ) ;
#12130 = DIRECTION ( 'NONE',  ( -0.000000000000000000, 1.000000000000000000, -0.000000000000000000 ) ) ;
#12131 = DIRECTION ( 'NONE',  ( 0.000000000000000000, 1.000000000000000000, 0.000000000000000000 ) ) ;
#12132 = CIRCLE ( 'NONE', #8336, 1.999999999999993117 ) ;
#12133 = CARTESIAN_POINT ( 'NONE',  ( -35.05918829505000645, -6.027090492554000534, 68.85549045786049760 ) ) ;
#12134 = ORIENTED_EDGE ( 'NONE', *, *, #11350, .T. ) ;
#12135 = EDGE_LOOP ( 'NONE', ( #11895, #13113, #2861, #2346 ) ) ;
#12136 = ADVANCED_FACE ( 'NONE', ( #6067 ), #3030, .T. ) ;
#12137 = ORIENTED_EDGE ( 'NONE', *, *, #5407, .F. ) ;
#12138 = VERTEX_POINT ( 'NONE', #3855 ) ;
#12139 = CARTESIAN_POINT ( 'NONE',  ( 92.63563590245421153, 99.03908161011133870, 20.00000000000000000 ) ) ;
#12140 = CARTESIAN_POINT ( 'NONE',  ( 109.1537879975201406, 115.4601262030644762, 20.00000000000000000 ) ) ;
#12141 = VERTEX_POINT ( 'NONE', #902 ) ;
#12142 = CARTESIAN_POINT ( 'NONE',  ( -6.000000000000000888, -12.00000000000000178, 7.000000000000000000 ) ) ;
#12143 = CARTESIAN_POINT ( 'NONE',  ( 27.50000000000001066, 0.000000000000000000, 29.99999999999999645 ) ) ;
#12144 = LINE ( 'NONE', #10974, #11767 ) ;
#12145 = DIRECTION ( 'NONE',  ( 0.000000000000000000, 0.000000000000000000, 1.000000000000000000 ) ) ;
#12146 = CARTESIAN_POINT ( 'NONE',  ( -7.999999999999998224, 2.000000000000000000, -65.00000000000000000 ) ) ;
#12147 = ORIENTED_EDGE ( 'NONE', *, *, #6132, .T. ) ;
#12148 = CARTESIAN_POINT ( 'NONE',  ( 8.000000000000000000, -1.762812401309176307E-15, 0.000000000000000000 ) ) ;
#12149 = DIRECTION ( 'NONE',  ( 1.000000000000000000, 0.000000000000000000, 0.000000000000000000 ) ) ;
#12150 = DIRECTION ( 'NONE',  ( 1.000000000000000000, -0.000000000000000000, -0.000000000000000000 ) ) ;
#12151 = DIRECTION ( 'NONE',  ( 0.000000000000000000, 0.000000000000000000, 1.000000000000000000 ) ) ;
#12152 = CARTESIAN_POINT ( 'NONE',  ( 109.1537879975201406, 82.61803701715820125, 0.7500000000000000000 ) ) ;
#12153 = EDGE_CURVE ( 'NONE', #3976, #10337, #11593, .T. ) ;
#12154 = VERTEX_POINT ( 'NONE', #8105 ) ;
#12155 = ORIENTED_EDGE ( 'NONE', *, *, #12814, .T. ) ;
#12156 = CYLINDRICAL_SURFACE ( 'NONE', #9497, 16.66282263685194920 ) ;
#12157 = EDGE_LOOP ( 'NONE', ( #13197, #11512, #13042, #7004 ) ) ;
#12158 = EDGE_LOOP ( 'NONE', ( #10167, #9186 ) ) ;
#12159 = DIRECTION ( 'NONE',  ( 1.000000000000000000, 0.000000000000000000, 0.000000000000000000 ) ) ;
#12160 = CARTESIAN_POINT ( 'NONE',  ( -0.5591882950499970084, 10.97290950744599947, 64.85000000000000853 ) ) ;
#12161 = DIRECTION ( 'NONE',  ( 0.000000000000000000, 0.000000000000000000, -1.000000000000000000 ) ) ;
#12162 = DIRECTION ( 'NONE',  ( 0.000000000000000000, -1.000000000000000000, 0.000000000000000000 ) ) ;
#12163 = CIRCLE ( 'NONE', #1441, 1.999999999999995781 ) ;
#12164 = CARTESIAN_POINT ( 'NONE',  ( 102.2760581142613603, 115.9375248198690826, 10.00000000000000000 ) ) ;
#12165 = DIRECTION ( 'NONE',  ( 1.000000000000000000, 0.000000000000000000, 0.000000000000000000 ) ) ;
#12166 = ORIENTED_EDGE ( 'NONE', *, *, #9622, .F. ) ;
#12167 = EDGE_CURVE ( 'NONE', #10920, #1440, #5995, .T. ) ;
#12168 = AXIS2_PLACEMENT_3D ( 'NONE', #3772, #5914, #1605 ) ;
#12169 = CARTESIAN_POINT ( 'NONE',  ( -17.92774181590637284, 30.36027202460865126, 61.70913974837020533 ) ) ;
#12170 = ORIENTED_EDGE ( 'NONE', *, *, #6435, .F. ) ;
#12171 = ORIENTED_EDGE ( 'NONE', *, *, #12908, .F. ) ;
#12172 = PRODUCT_DEFINITION_SHAPE ( 'NONE', 'NONE',  #13806 ) ;
#12173 = EDGE_LOOP ( 'NONE', ( #7779, #3307, #6272, #771 ) ) ;
#12174 = CARTESIAN_POINT ( 'NONE',  ( -18.05918829504999934, 10.97290950744599947, 62.14999999999999858 ) ) ;
#12175 = DIRECTION ( 'NONE',  ( 0.000000000000000000, 0.000000000000000000, 1.000000000000000000 ) ) ;
#12176 = VERTEX_POINT ( 'NONE', #8168 ) ;
#12177 = DIRECTION ( 'NONE',  ( 0.000000000000000000, -0.000000000000000000, -1.000000000000000000 ) ) ;
#12178 = DIRECTION ( 'NONE',  ( 1.000000000000000000, 0.000000000000000000, 0.000000000000000000 ) ) ;
#12179 = CARTESIAN_POINT ( 'NONE',  ( -18.05918829504999934, 10.97290950744599947, 27.09999999999999787 ) ) ;
#12180 = CIRCLE ( 'NONE', #3706, 16.75000000000000355 ) ;
#12181 = LINE ( 'NONE', #6794, #8467 ) ;
#12182 = EDGE_LOOP ( 'NONE', ( #4488, #9376, #6123, #1429 ) ) ;
#12183 = EDGE_CURVE ( 'NONE', #939, #6125, #9292, .T. ) ;
#12184 = AXIS2_PLACEMENT_3D ( 'NONE', #7632, #913, #7983 ) ;
#12185 = EDGE_CURVE ( 'NONE', #8674, #1279, #8653, .T. ) ;
#12186 = CARTESIAN_POINT ( 'NONE',  ( -18.05918829504999934, 10.97290950744599947, 57.35000000000000142 ) ) ;
#12187 = ORIENTED_EDGE ( 'NONE', *, *, #2361, .F. ) ;
#12188 = CYLINDRICAL_SURFACE ( 'NONE', #3302, 24.03999999999999915 ) ;
#12189 = ADVANCED_FACE ( 'NONE', ( #7179 ), #11939, .T. ) ;
#12190 = CARTESIAN_POINT ( 'NONE',  ( -21.53863742889154409, 30.09823897630959522, 55.53674328751647948 ) ) ;
#12191 = CARTESIAN_POINT ( 'NONE',  ( 109.6856792294029219, 82.08927268643400055, 20.00000000000000000 ) ) ;
#12192 = CARTESIAN_POINT ( 'NONE',  ( 1.629816981350590055, -4.941769416738769571, 17.25000000000000000 ) ) ;
#12193 = DIRECTION ( 'NONE',  ( 0.000000000000000000, 0.000000000000000000, 1.000000000000000000 ) ) ;
#12194 = DIRECTION ( 'NONE',  ( -0.7050191076322684935, 0.7091883091770477821, 0.000000000000000000 ) ) ;
#12195 = DIRECTION ( 'NONE',  ( 1.000000000000000000, 0.000000000000000000, 0.000000000000000000 ) ) ;
#12196 = DIRECTION ( 'NONE',  ( 0.000000000000000000, 0.000000000000000000, 1.000000000000000000 ) ) ;
#12197 = EDGE_LOOP ( 'NONE', ( #8234, #6514 ) ) ;
#12198 = VERTEX_POINT ( 'NONE', #3429 ) ;
#12199 = CIRCLE ( 'NONE', #9739, 6.000000000000000888 ) ;
#12200 = EDGE_CURVE ( 'NONE', #12616, #6439, #5979, .T. ) ;
#12201 = CARTESIAN_POINT ( 'NONE',  ( -15.34212233881444831, 16.32244711264754855, 60.04999999999999716 ) ) ;
#12202 = FACE_OUTER_BOUND ( 'NONE', #6139, .T. ) ;
#12203 = DIRECTION ( 'NONE',  ( 0.000000000000000000, 0.000000000000000000, 1.000000000000000000 ) ) ;
#12204 = DIRECTION ( 'NONE',  ( 0.6615960714621564875, -0.7498604124941129490, 0.000000000000000000 ) ) ;
#12205 = CIRCLE ( 'NONE', #8627, 6.000000000000000888 ) ;
#12206 = EDGE_CURVE ( 'NONE', #7886, #13749, #11726, .T. ) ;
#12207 = CARTESIAN_POINT ( 'NONE',  ( -3.499999999999998224, 2.499999999999999556, -65.00000000000000000 ) ) ;
#12208 = DIRECTION ( 'NONE',  ( 0.000000000000000000, 0.000000000000000000, -1.000000000000000000 ) ) ;
#12209 = DIRECTION ( 'NONE',  ( 0.000000000000000000, 0.000000000000000000, 1.000000000000000000 ) ) ;
#12210 = VERTEX_POINT ( 'NONE', #8641 ) ;
#12211 = DIRECTION ( 'NONE',  ( -1.000000000000000000, 0.000000000000000000, 0.000000000000000000 ) ) ;
#12212 = CARTESIAN_POINT ( 'NONE',  ( -35.05918829505000645, -6.027090492554000534, 7.250000000000000000 ) ) ;
#12213 = PLANE ( 'NONE',  #9172 ) ;
#12214 = CARTESIAN_POINT ( 'NONE',  ( -18.05918829504999934, 10.97290950744599947, 60.04999999999999716 ) ) ;
#12215 = CARTESIAN_POINT ( 'NONE',  ( -1.059188295050000894, 10.97290950744599947, 12.50000000000000000 ) ) ;
#12216 = AXIS2_PLACEMENT_3D ( 'NONE', #13166, #5889, #12466 ) ;
#12217 = ORIENTED_EDGE ( 'NONE', *, *, #7150, .T. ) ;
#12218 = CARTESIAN_POINT ( 'NONE',  ( 6.000000000000000888, 0.000000000000000000, 0.000000000000000000 ) ) ;
#12219 = ORIENTED_EDGE ( 'NONE', *, *, #10035, .F. ) ;
#12220 = ORIENTED_EDGE ( 'NONE', *, *, #11835, .F. ) ;
#12221 = DIRECTION ( 'NONE',  ( 0.4528443260392608360, 0.8915896008669277339, 0.000000000000000000 ) ) ;
#12222 = EDGE_CURVE ( 'NONE', #135, #8835, #4194, .T. ) ;
#12223 = LINE ( 'NONE', #13330, #9 ) ;
#12224 = AXIS2_PLACEMENT_3D ( 'NONE', #13097, #2645, #6875 ) ;
#12225 = FACE_OUTER_BOUND ( 'NONE', #7287, .T. ) ;
#12226 = AXIS2_PLACEMENT_3D ( 'NONE', #9855, #13045, #6760 ) ;
#12227 = CARTESIAN_POINT ( 'NONE',  ( -1.059188295049996231, 27.97290950744599769, 5.250000000000000000 ) ) ;
#12228 = VECTOR ( 'NONE', #8342, 1000.000000000000000 ) ;
#12229 = FACE_BOUND ( 'NONE', #4753, .T. ) ;
#12230 = CARTESIAN_POINT ( 'NONE',  ( -18.05918829504999934, 10.97290950744599947, 67.84999999999999432 ) ) ;
#12231 = DIRECTION ( 'NONE',  ( 1.000000000000000000, 0.000000000000000000, 0.000000000000000000 ) ) ;
#12232 = CIRCLE ( 'NONE', #5297, 1.999999999999996669 ) ;
#12233 = TOROIDAL_SURFACE ( 'NONE', #11347, 10.00000000000000000, 2.000000000000000000 ) ;
#12234 = AXIS2_PLACEMENT_3D ( 'NONE', #11317, #7110, #3087 ) ;
#12235 = AXIS2_PLACEMENT_3D ( 'NONE', #4975, #3795, #10157 ) ;
#12236 = EDGE_LOOP ( 'NONE', ( #9269, #8582, #9151, #9650 ) ) ;
#12237 = CARTESIAN_POINT ( 'NONE',  ( -16.82673727123299301, 30.32761401379713817, 61.47513517491817936 ) ) ;
#12238 = EDGE_LOOP ( 'NONE', ( #4984, #7121, #10334, #1701 ) ) ;
#12239 = VERTEX_POINT ( 'NONE', #6486 ) ;
#12240 = CARTESIAN_POINT ( 'NONE',  ( -18.05918829504999934, 10.97290950744599947, 30.59999999999999787 ) ) ;
#12241 = VERTEX_POINT ( 'NONE', #6617 ) ;
#12242 = DIRECTION ( 'NONE',  ( 0.000000000000000000, 0.000000000000000000, -1.000000000000000000 ) ) ;
#12243 = FACE_OUTER_BOUND ( 'NONE', #5913, .T. ) ;
#12244 = DIRECTION ( 'NONE',  ( 0.000000000000000000, -0.000000000000000000, 1.000000000000000000 ) ) ;
#12245 = ORIENTED_EDGE ( 'NONE', *, *, #5498, .T. ) ;
#12246 = CARTESIAN_POINT ( 'NONE',  ( -35.05918829505000645, -6.027090492554000534, 0.000000000000000000 ) ) ;
#12247 = CIRCLE ( 'NONE', #13353, 0.7499999999999966693 ) ;
#12248 = DIRECTION ( 'NONE',  ( 1.000000000000000000, 0.000000000000000000, 0.000000000000000000 ) ) ;
#12249 = ADVANCED_FACE ( 'NONE', ( #7656 ), #60, .F. ) ;
#12250 = CIRCLE ( 'NONE', #13781, 0.7500000000000006661 ) ;
#12251 = LINE ( 'NONE', #4570, #4457 ) ;
#12252 = ADVANCED_FACE ( 'NONE', ( #9641 ), #121, .T. ) ;
#12253 = VECTOR ( 'NONE', #7638, 999.9999999999998863 ) ;
#12254 = LINE ( 'NONE', #7134, #5802 ) ;
#12255 = ORIENTED_EDGE ( 'NONE', *, *, #10795, .T. ) ;
#12256 = EDGE_CURVE ( 'NONE', #223, #1784, #7748, .T. ) ;
#12257 = ORIENTED_EDGE ( 'NONE', *, *, #4279, .F. ) ;
#12258 = DIRECTION ( 'NONE',  ( -1.000000000000000000, -0.000000000000000000, -0.000000000000000000 ) ) ;
#12259 = ORIENTED_EDGE ( 'NONE', *, *, #11392, .F. ) ;
#12260 = VERTEX_POINT ( 'NONE', #2249 ) ;
#12261 = CARTESIAN_POINT ( 'NONE',  ( -10.22585496205000055, 10.97290950744599947, 60.04999999999999716 ) ) ;
#12262 = ORIENTED_EDGE ( 'NONE', *, *, #13673, .T. ) ;
#12263 = DIRECTION ( 'NONE',  ( 1.000000000000000000, 0.000000000000000000, 0.000000000000000000 ) ) ;
#12264 = CARTESIAN_POINT ( 'NONE',  ( -20.84908644685638279, 30.19213140065619783, 54.37388926677692780 ) ) ;
#12265 = DIRECTION ( 'NONE',  ( 0.4528443260392608360, 0.8915896008669278450, 0.000000000000000000 ) ) ;
#12266 = DIRECTION ( 'NONE',  ( 1.000000000000000000, 0.000000000000000000, 0.000000000000000000 ) ) ;
#12267 = LINE ( 'NONE', #9324, #1276 ) ;
#12268 = CARTESIAN_POINT ( 'NONE',  ( 76.11748380738829667, 82.61803701715820125, 0.7500000000000000000 ) ) ;
#12269 = ADVANCED_FACE ( 'NONE', ( #10754 ), #4394, .T. ) ;
#12270 = DIRECTION ( 'NONE',  ( 1.000000000000000000, 0.000000000000000000, 0.000000000000000000 ) ) ;
#12271 = DIRECTION ( 'NONE',  ( 1.000000000000000000, 0.000000000000000000, 0.000000000000000000 ) ) ;
#12272 = VERTEX_POINT ( 'NONE', #12981 ) ;
#12273 = EDGE_CURVE ( 'NONE', #1420, #5251, #6201, .T. ) ;
#12274 = EDGE_CURVE ( 'NONE', #12691, #7749, #12903, .T. ) ;
#12275 = DIRECTION ( 'NONE',  ( 0.6615960714621568206, -0.7498604124941125049, 0.000000000000000000 ) ) ;
#12276 = CARTESIAN_POINT ( 'NONE',  ( 2.262399129208279902, 22.44393519180574970, 17.25000000000000000 ) ) ;
#12277 = ORIENTED_EDGE ( 'NONE', *, *, #2732, .F. ) ;
#12278 = CARTESIAN_POINT ( 'NONE',  ( -1.059188295049996231, -6.027090492554000534, 10.00000000000000000 ) ) ;
#12279 = CARTESIAN_POINT ( 'NONE',  ( 44.63563590245422574, 113.0390816101113387, 19.25000000000000000 ) ) ;
#12280 = CARTESIAN_POINT ( 'NONE',  ( -35.05918829505000645, 27.97290950744599769, 5.250000000000000000 ) ) ;
#12281 = CARTESIAN_POINT ( 'NONE',  ( -28.87730642030694739, -7.867426463707980488, 17.25000000000000000 ) ) ;
#12282 = AXIS2_PLACEMENT_3D ( 'NONE', #603, #11294, #537 ) ;
#12283 = AXIS2_PLACEMENT_3D ( 'NONE', #9653, #7665, #1111 ) ;
#12284 = CIRCLE ( 'NONE', #8261, 16.66282263685194920 ) ;
#12285 = CARTESIAN_POINT ( 'NONE',  ( -22.21635405521520923, 13.97298182380577281, 68.75391885985828822 ) ) ;
#12286 = DIRECTION ( 'NONE',  ( -1.000000000000000000, 0.000000000000000000, 0.000000000000000000 ) ) ;
#12287 = AXIS2_PLACEMENT_3D ( 'NONE', #2250, #7798, #10493 ) ;
#12288 = CARTESIAN_POINT ( 'NONE',  ( -35.05918829505000645, 27.97290950744599769, 64.35000000000000853 ) ) ;
#12289 = CARTESIAN_POINT ( 'NONE',  ( 109.6856792294029219, 82.08927268643400055, 0.7500000000000006661 ) ) ;
#12290 = ADVANCED_FACE ( 'NONE', ( #12831 ), #2174, .F. ) ;
#12291 = CARTESIAN_POINT ( 'NONE',  ( 3.940811704950003325, 35.97290950744599058, 0.000000000000000000 ) ) ;
#12292 = DIRECTION ( 'NONE',  ( 0.000000000000000000, 0.000000000000000000, 1.000000000000000000 ) ) ;
#12293 = EDGE_CURVE ( 'NONE', #8888, #5295, #6411, .T. ) ;
#12294 = EDGE_CURVE ( 'NONE', #11638, #3446, #9801, .T. ) ;
#12295 = AXIS2_PLACEMENT_3D ( 'NONE', #7557, #11978, #11845 ) ;
#12296 = CIRCLE ( 'NONE', #8041, 1.499999999999999556 ) ;
#12297 = CIRCLE ( 'NONE', #3597, 3.000000000000002665 ) ;
#12298 = VECTOR ( 'NONE', #2534, 1000.000000000000000 ) ;
#12299 = VERTEX_POINT ( 'NONE', #1594 ) ;
#12300 = ORIENTED_EDGE ( 'NONE', *, *, #11350, .F. ) ;
#12301 = PLANE ( 'NONE',  #13274 ) ;
#12302 = VERTEX_POINT ( 'NONE', #10977 ) ;
#12303 = CARTESIAN_POINT ( 'NONE',  ( -35.05918829505000645, 27.97290950744599769, 0.000000000000000000 ) ) ;
#12304 = CARTESIAN_POINT ( 'NONE',  ( -10.25088531517539892, 30.80589556422609832, 5.250000000000000000 ) ) ;
#12305 = FACE_BOUND ( 'NONE', #1797, .T. ) ;
#12306 = DIRECTION ( 'NONE',  ( 0.000000000000000000, 0.000000000000000000, 1.000000000000000000 ) ) ;
#12307 = ADVANCED_FACE ( 'NONE', ( #13254 ), #2738, .T. ) ;
#12308 = AXIS2_PLACEMENT_3D ( 'NONE', #9789, #1112, #5238 ) ;
#12309 = SHAPE_REPRESENTATION ( 'Central Rotary Housing', ( #6434 ), #5310 ) ;
#12310 = AXIS2_PLACEMENT_3D ( 'NONE', #7540, #8471, #10857 ) ;
#12311 = CARTESIAN_POINT ( 'NONE',  ( 134.6356359024541973, 94.65549801902425031, 23.00000000000000000 ) ) ;
#12312 = AXIS2_PLACEMENT_3D ( 'NONE', #175, #5414, #9691 ) ;
#12313 = DIRECTION ( 'NONE',  ( -0.000000000000000000, 1.000000000000000000, -0.000000000000000000 ) ) ;
#12314 = PLANE ( 'NONE',  #4261 ) ;
#12315 = EDGE_CURVE ( 'NONE', #10428, #4952, #4746, .T. ) ;
#12316 = VERTEX_POINT ( 'NONE', #277 ) ;
#12317 = CARTESIAN_POINT ( 'NONE',  ( -1.059188295049996231, 27.97290950744599769, 64.35000000000000853 ) ) ;
#12318 = CIRCLE ( 'NONE', #6289, 23.29163056034261459 ) ;
#12319 = EDGE_LOOP ( 'NONE', ( #9876, #11840, #10692, #5443 ) ) ;
#12320 = ORIENTED_EDGE ( 'NONE', *, *, #350, .F. ) ;
#12321 = LINE ( 'NONE', #1622, #1461 ) ;
#12322 = VERTEX_POINT ( 'NONE', #3638 ) ;
#12323 = FACE_OUTER_BOUND ( 'NONE', #13275, .T. ) ;
#12324 = ORIENTED_EDGE ( 'NONE', *, *, #8339, .F. ) ;
#12325 = CARTESIAN_POINT ( 'NONE',  ( -18.05918829504999934, 18.59295644444599915, 61.63595870800000398 ) ) ;
#12326 = CARTESIAN_POINT ( 'NONE',  ( -12.26420230435512160, 9.417873376788568507, 68.84999999999999432 ) ) ;
#12327 = CARTESIAN_POINT ( 'NONE',  ( 2.262399129208274573, -0.4981161769137525952, 83.57661607529820458 ) ) ;
#12328 = DIRECTION ( 'NONE',  ( 0.000000000000000000, 0.000000000000000000, -1.000000000000000000 ) ) ;
#12329 = CARTESIAN_POINT ( 'NONE',  ( -38.38077571930825371, -0.4981161769137670281, 17.25000000000000000 ) ) ;
#12330 = CARTESIAN_POINT ( 'NONE',  ( -18.05918829504999934, 10.97290950744599947, 64.85000000000000853 ) ) ;
#12331 = CIRCLE ( 'NONE', #6064, 17.00000000000000000 ) ;
#12332 = ORIENTED_EDGE ( 'NONE', *, *, #9645, .F. ) ;
#12333 = EDGE_LOOP ( 'NONE', ( #10009, #8603 ) ) ;
#12334 = ORIENTED_EDGE ( 'NONE', *, *, #206, .F. ) ;
#12335 = EDGE_CURVE ( 'NONE', #3979, #11332, #13048, .T. ) ;
#12336 = EDGE_LOOP ( 'NONE', ( #1781, #9790 ) ) ;
#12337 = ORIENTED_EDGE ( 'NONE', *, *, #9533, .T. ) ;
#12338 = CARTESIAN_POINT ( 'NONE',  ( 16.08092853089229024, 4.500000000000000000, -7.237812082545202585 ) ) ;
#12339 = ORIENTED_EDGE ( 'NONE', *, *, #36, .F. ) ;
#12340 = CARTESIAN_POINT ( 'NONE',  ( -19.63224265096508958, 30.30694957903927644, 61.32011773191905490 ) ) ;
#12341 = FACE_OUTER_BOUND ( 'NONE', #8337, .T. ) ;
#12342 = DIRECTION ( 'NONE',  ( 0.000000000000000000, 0.000000000000000000, 1.000000000000000000 ) ) ;
#12343 = CARTESIAN_POINT ( 'NONE',  ( -18.05918829504999934, 10.97290950744599947, 68.84999999999999432 ) ) ;
#12344 = DIRECTION ( 'NONE',  ( 0.000000000000000000, 0.000000000000000000, 1.000000000000000000 ) ) ;
#12345 = AXIS2_PLACEMENT_3D ( 'NONE', #9466, #5255, #10579 ) ;
#12346 = ADVANCED_FACE ( 'NONE', ( #8857 ), #7307, .T. ) ;
#12347 = ORIENTED_EDGE ( 'NONE', *, *, #1207, .T. ) ;
#12348 = CARTESIAN_POINT ( 'NONE',  ( -23.24102627739274851, -6.265087914666289670, 62.14999999999999858 ) ) ;
#12349 = ORIENTED_EDGE ( 'NONE', *, *, #8220, .T. ) ;
#12350 = ORIENTED_EDGE ( 'NONE', *, *, #10998, .F. ) ;
#12351 = DIRECTION ( 'NONE',  ( 0.000000000000000000, 0.000000000000000000, 1.000000000000000000 ) ) ;
#12352 = DIRECTION ( 'NONE',  ( -0.000000000000000000, 1.000000000000000000, -0.000000000000000000 ) ) ;
#12353 = DIRECTION ( 'NONE',  ( 0.000000000000000000, 0.000000000000000000, -1.000000000000000000 ) ) ;
#12354 = AXIS2_PLACEMENT_3D ( 'NONE', #7257, #124, #10823 ) ;
#12355 = CARTESIAN_POINT ( 'NONE',  ( 4.500000000000002665, -4.336808689942017736E-16, -65.00000000000000000 ) ) ;
#12356 = DIRECTION ( 'NONE',  ( 0.000000000000000000, 0.000000000000000000, 1.000000000000000000 ) ) ;
#12357 = CARTESIAN_POINT ( 'NONE',  ( -35.05918829505000645, 27.97290950744599769, 64.35000000000000853 ) ) ;
#12358 = CYLINDRICAL_SURFACE ( 'NONE', #1312, 0.2500000000000002220 ) ;
#12359 = CARTESIAN_POINT ( 'NONE',  ( -27.49999999999998934, 0.000000000000000000, -30.00000000000000355 ) ) ;
#12360 = CARTESIAN_POINT ( 'NONE',  ( -24.20502162805000168, 10.97290950744599947, 60.60999999999999943 ) ) ;
#12361 = DIRECTION ( 'NONE',  ( 0.000000000000000000, 0.000000000000000000, -1.000000000000000000 ) ) ;
#12362 = EDGE_LOOP ( 'NONE', ( #5422, #6987, #8271, #12655, #1621, #4722, #5402, #1242 ) ) ;
#12363 = EDGE_CURVE ( 'NONE', #363, #939, #7937, .T. ) ;
#12364 = CARTESIAN_POINT ( 'NONE',  ( -37.75918829505000218, 27.97290950744599769, 58.85000000000000142 ) ) ;
#12365 = ORIENTED_EDGE ( 'NONE', *, *, #10553, .T. ) ;
#12366 = ORIENTED_EDGE ( 'NONE', *, *, #13723, .F. ) ;
#12367 = FACE_OUTER_BOUND ( 'NONE', #12370, .T. ) ;
#12368 = CARTESIAN_POINT ( 'NONE',  ( 42.63563590245419732, 112.2890816101113387, 0.7500000000000006661 ) ) ;
#12369 = CARTESIAN_POINT ( 'NONE',  ( -18.45469220996244886, -1.832421873814834123, -3.000000000000000000 ) ) ;
#12370 = EDGE_LOOP ( 'NONE', ( #2481, #4125, #201, #619 ) ) ;
#12371 = DIRECTION ( 'NONE',  ( 0.3984948954980490621, -4.880154982482439852E-17, 0.9171705502587831349 ) ) ;
#12372 = EDGE_CURVE ( 'NONE', #11621, #11264, #3763, .T. ) ;
#12373 = CARTESIAN_POINT ( 'NONE',  ( -38.38077571930825371, 22.44393519180574970, 5.250000000000000000 ) ) ;
#12374 = DIRECTION ( 'NONE',  ( 0.000000000000000000, 0.000000000000000000, 1.000000000000000000 ) ) ;
#12375 = CARTESIAN_POINT ( 'NONE',  ( -35.05918829505000645, -6.027090492554000534, 83.57661607529820458 ) ) ;
#12376 = ORIENTED_EDGE ( 'NONE', *, *, #7438, .F. ) ;
#12377 = EDGE_CURVE ( 'NONE', #4651, #12584, #9110, .T. ) ;
#12378 = ORIENTED_EDGE ( 'NONE', *, *, #9365, .T. ) ;
#12379 = CARTESIAN_POINT ( 'NONE',  ( -17.59482673585142365, 30.35570588519015445, 61.67721350625757282 ) ) ;
#12380 = VERTEX_POINT ( 'NONE', #8013 ) ;
#12381 = CARTESIAN_POINT ( 'NONE',  ( -18.05918829505000645, 3.394200320306482332, 61.95399527338132373 ) ) ;
#12382 = ORIENTED_EDGE ( 'NONE', *, *, #9933, .T. ) ;
#12383 = CARTESIAN_POINT ( 'NONE',  ( -18.45469220996244886, -1.832421873814834123, 0.000000000000000000 ) ) ;
#12384 = DIRECTION ( 'NONE',  ( 1.000000000000000000, 0.000000000000000000, 0.000000000000000000 ) ) ;
#12385 = ORIENTED_EDGE ( 'NONE', *, *, #11252, .T. ) ;
#12386 = ADVANCED_FACE ( 'NONE', ( #2664 ), #2884, .F. ) ;
#12387 = DIRECTION ( 'NONE',  ( 0.000000000000000000, 0.000000000000000000, 1.000000000000000000 ) ) ;
#12388 = FACE_OUTER_BOUND ( 'NONE', #8079, .T. ) ;
#12389 = LINE ( 'NONE', #7062, #876 ) ;
#12390 = DIRECTION ( 'NONE',  ( -0.7071067811865524577, -0.7071067811865425767, 0.000000000000000000 ) ) ;
#12391 = AXIS2_PLACEMENT_3D ( 'NONE', #4703, #10150, #3788 ) ;
#12392 = EDGE_LOOP ( 'NONE', ( #6103, #6153, #12366, #9537 ) ) ;
#12393 = ORIENTED_EDGE ( 'NONE', *, *, #9126, .T. ) ;
#12394 = VERTEX_POINT ( 'NONE', #543 ) ;
#12395 = ORIENTED_EDGE ( 'NONE', *, *, #8442, .F. ) ;
#12396 = CYLINDRICAL_SURFACE ( 'NONE', #1748, 24.92993838181874722 ) ;
#12397 = ADVANCED_FACE ( 'NONE', ( #5638 ), #3492, .T. ) ;
#12398 = DIRECTION ( 'NONE',  ( 1.000000000000000000, 0.000000000000000000, 0.000000000000000000 ) ) ;
#12399 = CARTESIAN_POINT ( 'NONE',  ( -32.35918829505000360, -6.027090492554000534, 7.250000000000000000 ) ) ;
#12400 = DIRECTION ( 'NONE',  ( 0.000000000000000000, -2.202823461557850341E-15, 1.000000000000000000 ) ) ;
#12401 = DIRECTION ( 'NONE',  ( 1.000000000000000000, 0.000000000000000000, 0.000000000000000000 ) ) ;
#12402 = FACE_OUTER_BOUND ( 'NONE', #5835, .T. ) ;
#12403 = DIRECTION ( 'NONE',  ( 4.597850203645602824E-29, -6.780744947014009727E-15, 1.000000000000000000 ) ) ;
#12404 = ADVANCED_FACE ( 'NONE', ( #2533 ), #9002, .T. ) ;
#12405 = ORIENTED_EDGE ( 'NONE', *, *, #13296, .T. ) ;
#12406 = DIRECTION ( 'NONE',  ( 0.000000000000000000, -0.000000000000000000, 1.000000000000000000 ) ) ;
#12407 = CARTESIAN_POINT ( 'NONE',  ( -28.87730642030694739, -7.867426463707978712, 83.57661607529820458 ) ) ;
#12408 = VERTEX_POINT ( 'NONE', #7723 ) ;
#12409 = DIRECTION ( 'NONE',  ( 0.000000000000000000, 0.000000000000000000, 1.000000000000000000 ) ) ;
#12410 = DIRECTION ( 'NONE',  ( 0.6615960714621565986, -0.7498604124941128379, 0.000000000000000000 ) ) ;
#12411 = DIRECTION ( 'NONE',  ( -1.000000000000000000, 0.000000000000000000, 0.000000000000000000 ) ) ;
#12412 = DIRECTION ( 'NONE',  ( 1.000000000000000000, 0.000000000000000000, 0.000000000000000000 ) ) ;
#12413 = DIRECTION ( 'NONE',  ( 0.000000000000000000, 1.000000000000000000, 0.000000000000000000 ) ) ;
#12414 = DIRECTION ( 'NONE',  ( 1.224646799147353207E-16, 1.000000000000000000, -0.000000000000000000 ) ) ;
#12415 = CARTESIAN_POINT ( 'NONE',  ( 92.63563590245421153, 99.03908161011133870, 20.00000000000000000 ) ) ;
#12416 = FACE_OUTER_BOUND ( 'NONE', #10217, .T. ) ;
#12417 = CIRCLE ( 'NONE', #3943, 8.300000000000000711 ) ;
#12418 = DIRECTION ( 'NONE',  ( 0.000000000000000000, 0.000000000000000000, 1.000000000000000000 ) ) ;
#12419 = EDGE_CURVE ( 'NONE', #9316, #10219, #341, .T. ) ;
#12420 = EDGE_CURVE ( 'NONE', #189, #826, #11036, .T. ) ;
#12421 = UNCERTAINTY_MEASURE_WITH_UNIT (LENGTH_MEASURE( 1.000000000000000082E-05 ), #5756, 'distance_accuracy_value', 'NONE');
#12422 = VERTEX_POINT ( 'NONE', #9982 ) ;
#12423 = EDGE_LOOP ( 'NONE', ( #11565, #7552 ) ) ;
#12424 = ORIENTED_EDGE ( 'NONE', *, *, #1008, .T. ) ;
#12425 = DIRECTION ( 'NONE',  ( 0.000000000000000000, 0.000000000000000000, 1.000000000000000000 ) ) ;
#12426 = EDGE_LOOP ( 'NONE', ( #9703, #11510, #9268, #13626 ) ) ;
#12427 = ORIENTED_EDGE ( 'NONE', *, *, #13592, .T. ) ;
#12428 = CARTESIAN_POINT ( 'NONE',  ( -20.73856204053882735, 15.27682634614306600, 68.78022907841716460 ) ) ;
#12429 = DIRECTION ( 'NONE',  ( 0.000000000000000000, 0.000000000000000000, 1.000000000000000000 ) ) ;
#12430 = SURFACE_STYLE_USAGE ( .BOTH. , #11047 ) ;
#12431 = LINE ( 'NONE', #13680, #6880 ) ;
#12432 = CARTESIAN_POINT ( 'NONE',  ( 50.63563590245420443, 108.9054980190242503, 23.00000000000000000 ) ) ;
#12433 = DIRECTION ( 'NONE',  ( -1.000000000000000000, 0.000000000000000000, 0.000000000000000000 ) ) ;
#12434 = EDGE_CURVE ( 'NONE', #5647, #6318, #407, .T. ) ;
#12435 = DIRECTION ( 'NONE',  ( 1.000000000000000000, 0.000000000000000000, 0.000000000000000000 ) ) ;
#12436 = ORIENTED_EDGE ( 'NONE', *, *, #8188, .F. ) ;
#12437 = ORIENTED_EDGE ( 'NONE', *, *, #9064, .T. ) ;
#12438 = CARTESIAN_POINT ( 'NONE',  ( -14.84085382869762881, 30.13625835401696307, 59.70232134295659421 ) ) ;
#12439 = CIRCLE ( 'NONE', #8645, 34.69999999999999574 ) ;
#12440 = ORIENTED_EDGE ( 'NONE', *, *, #559, .T. ) ;
#12441 = EDGE_LOOP ( 'NONE', ( #3502, #4015, #7116, #13351, #10665, #790, #2261, #3878, #11733, #8916, #702, #3975, #1686, #4969, #4816 ) ) ;
#12442 = CIRCLE ( 'NONE', #2431, 16.00000000000000000 ) ;
#12443 = SURFACE_STYLE_USAGE ( .BOTH. , #13423 ) ;
#12444 = CARTESIAN_POINT ( 'NONE',  ( -1.059188295049996231, 27.97290950744599769, 10.00000000000000000 ) ) ;
#12445 = EDGE_LOOP ( 'NONE', ( #10294, #4863, #6786, #4264 ) ) ;
#12446 = ORIENTED_EDGE ( 'NONE', *, *, #13140, .F. ) ;
#12447 = CARTESIAN_POINT ( 'NONE',  ( -14.08961186627706041, 6.473747032481329988, 68.84999999999999432 ) ) ;
#12448 = CARTESIAN_POINT ( 'NONE',  ( -40.05918829504999934, -14.02709049255400053, 10.00000000000000000 ) ) ;
#12449 = LINE ( 'NONE', #10297, #11170 ) ;
#12450 = DIRECTION ( 'NONE',  ( 0.000000000000000000, 0.000000000000000000, 1.000000000000000000 ) ) ;
#12451 = CARTESIAN_POINT ( 'NONE',  ( -16.59761566455133774, 27.91013588845822468, 57.74153177338070009 ) ) ;
#12452 = EDGE_CURVE ( 'NONE', #7749, #9802, #11779, .T. ) ;
#12453 = DIRECTION ( 'NONE',  ( 0.4528443260392608916, 0.8915896008669277339, 0.000000000000000000 ) ) ;
#12454 = CIRCLE ( 'NONE', #8880, 6.145833333000000565 ) ;
#12455 = AXIS2_PLACEMENT_3D ( 'NONE', #1172, #11873, #10892 ) ;
#12456 = AXIS2_PLACEMENT_3D ( 'NONE', #8469, #1002, #4299 ) ;
#12457 = EDGE_CURVE ( 'NONE', #7434, #11514, #13774, .T. ) ;
#12458 = EDGE_LOOP ( 'NONE', ( #9993, #8352, #6467, #11912, #11997 ) ) ;
#12459 = EDGE_CURVE ( 'NONE', #651, #7262, #1524, .T. ) ;
#12460 = VERTEX_POINT ( 'NONE', #6182 ) ;
#12461 = ORIENTED_EDGE ( 'NONE', *, *, #1540, .T. ) ;
#12462 = AXIS2_PLACEMENT_3D ( 'NONE', #3103, #4974, #8180 ) ;
#12463 = EDGE_LOOP ( 'NONE', ( #3700, #1165, #1382, #6297 ) ) ;
#12465 = ORIENTED_EDGE ( 'NONE', *, *, #12551, .F. ) ;
#12464 = TOROIDAL_SURFACE ( 'NONE', #5989, 10.75000000000000000, 0.7500000000000000000 ) ;
#12466 = DIRECTION ( 'NONE',  ( 1.000000000000000000, 0.000000000000000000, 0.000000000000000000 ) ) ;
#12467 = CARTESIAN_POINT ( 'NONE',  ( -20.58011868346011042, 30.22311051615698929, 60.62245744008113491 ) ) ;
#12468 = CARTESIAN_POINT ( 'NONE',  ( -18.05918829504999934, 10.97290950744599947, 60.60999999999999943 ) ) ;
#12469 = CARTESIAN_POINT ( 'NONE',  ( -7.499999999999996447, -0.5000000000000017764, 0.000000000000000000 ) ) ;
#12470 = CYLINDRICAL_SURFACE ( 'NONE', #13414, 1.999999999999991340 ) ;
#12471 = FACE_BOUND ( 'NONE', #7631, .T. ) ;
#12472 = CARTESIAN_POINT ( 'NONE',  ( -146.9091882950500576, 0.000000000000000000, 70.79081170495001629 ) ) ;
#12473 = EDGE_LOOP ( 'NONE', ( #6296, #5816 ) ) ;
#12474 = CIRCLE ( 'NONE', #6664, 1.500000000000001332 ) ;
#12475 = EDGE_CURVE ( 'NONE', #10489, #826, #5746, .T. ) ;
#12476 = CARTESIAN_POINT ( 'NONE',  ( 68.49370948373500312, 123.0390816101113245, 20.00000000000000000 ) ) ;
#12477 = ORIENTED_EDGE ( 'NONE', *, *, #2127, .F. ) ;
#12478 = ORIENTED_EDGE ( 'NONE', *, *, #12613, .F. ) ;
#12479 = CARTESIAN_POINT ( 'NONE',  ( -10.79835982676942052, -4.028726038184999858, 62.14999999999999858 ) ) ;
#12480 = LINE ( 'NONE', #8144, #12861 ) ;
#12481 = DIRECTION ( 'NONE',  ( 0.4528443260392608916, 0.8915896008669277339, 0.000000000000000000 ) ) ;
#12482 = CARTESIAN_POINT ( 'NONE',  ( -10.38347696868452097, 26.08535324214045303, 57.35000000000000142 ) ) ;
#12483 = DIRECTION ( 'NONE',  ( 0.000000000000000000, 0.000000000000000000, 1.000000000000000000 ) ) ;
#12484 = DIRECTION ( 'NONE',  ( -0.000000000000000000, -1.000000000000000000, -0.000000000000000000 ) ) ;
#12485 = DIRECTION ( 'NONE',  ( -0.000000000000000000, -0.000000000000000000, 1.000000000000000000 ) ) ;
#12486 = CARTESIAN_POINT ( 'NONE',  ( 140.6356359024541973, 108.9054980190242503, 22.75000000000000000 ) ) ;
#12487 = AXIS2_PLACEMENT_3D ( 'NONE', #11338, #3876, #4085 ) ;
#12488 = CARTESIAN_POINT ( 'NONE',  ( 50.38563590245420443, 108.6554980190242503, 23.00000000000000000 ) ) ;
#12489 = CIRCLE ( 'NONE', #13154, 6.450000000000009948 ) ;
#12490 = ADVANCED_FACE ( 'NONE', ( #13391 ), #12624, .F. ) ;
#12491 = VERTEX_POINT ( 'NONE', #11370 ) ;
#12492 = AXIS2_PLACEMENT_3D ( 'NONE', #3989, #6979, #10405 ) ;
#12493 = CARTESIAN_POINT ( 'NONE',  ( 86.99521369064697751, 82.14063840035363739, 10.00000000000000000 ) ) ;
#12494 = ORIENTED_EDGE ( 'NONE', *, *, #2482, .T. ) ;
#12495 = VECTOR ( 'NONE', #3462, 1000.000000000000000 ) ;
#12496 = EDGE_CURVE ( 'NONE', #1821, #11264, #3316, .T. ) ;
#12497 = ADVANCED_FACE ( 'NONE', ( #11301 ), #5973, .T. ) ;
#12498 = ORIENTED_EDGE ( 'NONE', *, *, #13629, .T. ) ;
#12499 = CARTESIAN_POINT ( 'NONE',  ( -21.25890827522755089, 14.81772886755349639, 68.85000000000002274 ) ) ;
#12500 = DIRECTION ( 'NONE',  ( 1.000000000000000000, 0.000000000000000000, 0.000000000000000000 ) ) ;
#12501 = FACE_OUTER_BOUND ( 'NONE', #2560, .T. ) ;
#12502 = DIRECTION ( 'NONE',  ( 0.000000000000000000, 0.000000000000000000, -1.000000000000000000 ) ) ;
#12503 = FACE_OUTER_BOUND ( 'NONE', #6027, .T. ) ;
#12504 = CARTESIAN_POINT ( 'NONE',  ( -35.05918829505000645, -6.027090492554000534, 64.85000000000000853 ) ) ;
#12505 = VECTOR ( 'NONE', #8786, 1000.000000000000114 ) ;
#12506 = AXIS2_PLACEMENT_3D ( 'NONE', #2755, #9071, #1742 ) ;
#12507 = AXIS2_PLACEMENT_3D ( 'NONE', #3299, #2128, #1989 ) ;
#12508 = AXIS2_PLACEMENT_3D ( 'NONE', #4634, #12112, #7128 ) ;
#12509 = EDGE_LOOP ( 'NONE', ( #4705, #4971, #4122, #1638 ) ) ;
#12510 = CARTESIAN_POINT ( 'NONE',  ( -14.39336303962373975, 30.06926057631024918, 56.09279642605752514 ) ) ;
#12511 = EDGE_LOOP ( 'NONE', ( #3532, #9724 ) ) ;
#12512 = EDGE_CURVE ( 'NONE', #209, #1798, #5539, .T. ) ;
#12513 = EDGE_LOOP ( 'NONE', ( #2570, #6158, #3484, #8499 ) ) ;
#12514 = CARTESIAN_POINT ( 'NONE',  ( 140.6356359024541973, 103.9054980190242361, 20.00000000000000000 ) ) ;
#12515 = AXIS2_PLACEMENT_3D ( 'NONE', #10091, #1288, #5544 ) ;
#12516 = DIRECTION ( 'NONE',  ( 0.3202092937642119774, 0.6304490528084089052, 0.7071067811865507924 ) ) ;
#12517 = CIRCLE ( 'NONE', #6492, 17.00000000000000355 ) ;
#12518 = FACE_OUTER_BOUND ( 'NONE', #12032, .T. ) ;
#12519 = CIRCLE ( 'NONE', #13182, 8.300000000000000711 ) ;
#12520 = VERTEX_POINT ( 'NONE', #11503 ) ;
#12521 = ADVANCED_FACE ( 'NONE', ( #1808 ), #6113, .F. ) ;
#12522 = CARTESIAN_POINT ( 'NONE',  ( -18.05918829504999934, 10.97290950744599947, 64.35000000000000853 ) ) ;
#12523 = FACE_OUTER_BOUND ( 'NONE', #12173, .T. ) ;
#12524 = ORIENTED_EDGE ( 'NONE', *, *, #7028, .T. ) ;
#12525 = FACE_OUTER_BOUND ( 'NONE', #2784, .T. ) ;
#12526 = DIRECTION ( 'NONE',  ( 1.000000000000000000, 0.000000000000000000, 0.000000000000000000 ) ) ;
#12527 = CARTESIAN_POINT ( 'NONE',  ( -25.86749127492454647, -8.860076549334129581, 17.25000000000000000 ) ) ;
#12528 = PRODUCT_RELATED_PRODUCT_CATEGORY ( 'part', '', ( #7628 ) ) ;
#12529 = FACE_OUTER_BOUND ( 'NONE', #6843, .T. ) ;
#12530 = CIRCLE ( 'NONE', #1367, 16.72262947720610171 ) ;
#12531 = AXIS2_PLACEMENT_3D ( 'NONE', #10805, #6465, #5269 ) ;
#12532 = CIRCLE ( 'NONE', #5826, 16.75000000000000355 ) ;
#12533 = EDGE_LOOP ( 'NONE', ( #5334, #9129, #2069, #11784 ) ) ;
#12534 = EDGE_LOOP ( 'NONE', ( #11188, #4102, #12839, #5369 ) ) ;
#12535 = EDGE_CURVE ( 'NONE', #11959, #9038, #4877, .T. ) ;
#12536 = ORIENTED_EDGE ( 'NONE', *, *, #2326, .F. ) ;
#12537 = EDGE_LOOP ( 'NONE', ( #1260, #4973, #2569, #7302 ) ) ;
#12538 = ORIENTED_EDGE ( 'NONE', *, *, #714, .T. ) ;
#12539 = DIRECTION ( 'NONE',  ( 0.000000000000000000, 0.000000000000000000, -1.000000000000000000 ) ) ;
#12540 = CARTESIAN_POINT ( 'NONE',  ( -19.61957230515337969, 30.30780693223203670, 61.32664748691393442 ) ) ;
#12541 = VECTOR ( 'NONE', #13742, 1000.000000000000000 ) ;
#12542 = ORIENTED_EDGE ( 'NONE', *, *, #6049, .F. ) ;
#12543 = CARTESIAN_POINT ( 'NONE',  ( 72.18094369249178044, 97.20665973629650125, 10.00000000000000000 ) ) ;
#12544 = LINE ( 'NONE', #4857, #4638 ) ;
#12545 = DIRECTION ( 'NONE',  ( 0.000000000000000000, 0.000000000000000000, -1.000000000000000000 ) ) ;
#12546 = ADVANCED_FACE ( 'NONE', ( #9137 ), #10386, .T. ) ;
#12547 = DIRECTION ( 'NONE',  ( -1.000000000000000000, 0.000000000000000000, -0.000000000000000000 ) ) ;
#12548 = DIRECTION ( 'NONE',  ( 1.000000000000000000, 0.000000000000000000, 0.000000000000000000 ) ) ;
#12549 = ORIENTED_EDGE ( 'NONE', *, *, #4865, .F. ) ;
#12550 = AXIS2_PLACEMENT_3D ( 'NONE', #2803, #8217, #11235 ) ;
#12551 = EDGE_CURVE ( 'NONE', #2380, #12422, #1660, .T. ) ;
#12552 = DIRECTION ( 'NONE',  ( 0.000000000000000000, 0.000000000000000000, -1.000000000000000000 ) ) ;
#12553 = PLANE ( 'NONE',  #8411 ) ;
#12554 = VERTEX_POINT ( 'NONE', #1878 ) ;
#12555 = CYLINDRICAL_SURFACE ( 'NONE', #3820, 13.50000000000000000 ) ;
#12556 = CARTESIAN_POINT ( 'NONE',  ( 44.63563590245421864, 85.03908161011133870, 20.00000000000000000 ) ) ;
#12557 = DIRECTION ( 'NONE',  ( 0.000000000000000000, 0.000000000000000000, -1.000000000000000000 ) ) ;
#12558 = PLANE ( 'NONE',  #10540 ) ;
#12559 = ORIENTED_EDGE ( 'NONE', *, *, #1915, .T. ) ;
#12560 = CARTESIAN_POINT ( 'NONE',  ( -34.05918829504999934, 10.97290950744599947, 7.250000000000000000 ) ) ;
#12561 = CARTESIAN_POINT ( 'NONE',  ( 50.38563590245420443, 90.15549801902423610, 23.00000000000000000 ) ) ;
#12562 = DIRECTION ( 'NONE',  ( 0.9576665234506833713, -0.2878798879079291217, 0.000000000000000000 ) ) ;
#12563 = EDGE_CURVE ( 'NONE', #7611, #10469, #861, .T. ) ;
#12564 = DIRECTION ( 'NONE',  ( -0.4528443260392610026, -0.8915896008669278450, 0.000000000000000000 ) ) ;
#12565 = DIRECTION ( 'NONE',  ( -0.7050191076322684935, -0.7091883091770477821, -0.000000000000000000 ) ) ;
#12566 = PRODUCT_DEFINITION_CONTEXT ( 'detailed design', #8845, 'design' ) ;
#12567 = ORIENTED_EDGE ( 'NONE', *, *, #2816, .T. ) ;
#12568 = VERTEX_POINT ( 'NONE', #12561 ) ;
#12569 = CIRCLE ( 'NONE', #5864, 6.049999999999999822 ) ;
#12570 = ORIENTED_EDGE ( 'NONE', *, *, #13055, .F. ) ;
#12571 = DIRECTION ( 'NONE',  ( 0.000000000000000000, 0.000000000000000000, -1.000000000000000000 ) ) ;
#12572 = ORIENTED_EDGE ( 'NONE', *, *, #490, .F. ) ;
#12573 = CARTESIAN_POINT ( 'NONE',  ( -21.36716865236079954, 14.72221156991656166, 68.84999999999999432 ) ) ;
#12574 = DIRECTION ( 'NONE',  ( -0.000000000000000000, -1.000000000000000000, -0.000000000000000000 ) ) ;
#12575 = LINE ( 'NONE', #10207, #5822 ) ;
#12576 = DIRECTION ( 'NONE',  ( -1.000000000000000000, 0.000000000000000000, 0.000000000000000000 ) ) ;
#12577 = ADVANCED_FACE ( 'NONE', ( #8150 ), #12358, .T. ) ;
#12578 = CARTESIAN_POINT ( 'NONE',  ( -29.51816008892539855, -2.179141222803619993, 62.14999999999999858 ) ) ;
#12579 = CIRCLE ( 'NONE', #5643, 6.595833333000001630 ) ;
#12580 = EDGE_CURVE ( 'NONE', #6443, #12635, #7766, .T. ) ;
#12581 = ORIENTED_EDGE ( 'NONE', *, *, #9411, .T. ) ;
#12582 = CARTESIAN_POINT ( 'NONE',  ( -14.42071735626405093, 30.07360145807300000, 55.99350896921582432 ) ) ;
#12583 = VERTEX_POINT ( 'NONE', #10192 ) ;
#12584 = VERTEX_POINT ( 'NONE', #10264 ) ;
#12585 = CARTESIAN_POINT ( 'NONE',  ( -8.500000000000000000, 2.499999999999999556, -65.00000000000000000 ) ) ;
#12586 = DIRECTION ( 'NONE',  ( 0.000000000000000000, 0.000000000000000000, 1.000000000000000000 ) ) ;
#12587 = CARTESIAN_POINT ( 'NONE',  ( -1.059188295049996231, -6.027090492554000534, 64.85000000000000853 ) ) ;
#12588 = ORIENTED_EDGE ( 'NONE', *, *, #3229, .T. ) ;
#12589 = ORIENTED_EDGE ( 'NONE', *, *, #7028, .F. ) ;
#12590 = DIRECTION ( 'NONE',  ( -1.000000000000000000, 1.239088197126291063E-16, -0.000000000000000000 ) ) ;
#12591 = DIRECTION ( 'NONE',  ( 0.000000000000000000, 1.000000000000000000, 0.000000000000000000 ) ) ;
#12592 = ORIENTED_EDGE ( 'NONE', *, *, #3088, .F. ) ;
#12593 = CARTESIAN_POINT ( 'NONE',  ( 116.7775623211734342, 113.0390816101113387, 19.25000000000000000 ) ) ;
#12594 = LINE ( 'NONE', #6226, #3874 ) ;
#12595 = CARTESIAN_POINT ( 'NONE',  ( -18.97946290528394186, 27.94856484295734234, 58.55107660166387262 ) ) ;
#12596 = STYLED_ITEM ( 'NONE', ( #3537 ), #229 ) ;
#12597 = LINE ( 'NONE', #7395, #3373 ) ;
#12598 = EDGE_CURVE ( 'NONE', #1146, #759, #4946, .T. ) ;
#12599 = EDGE_LOOP ( 'NONE', ( #11174, #1079, #13162, #9910 ) ) ;
#12600 = ORIENTED_EDGE ( 'NONE', *, *, #9214, .F. ) ;
#12601 = EDGE_LOOP ( 'NONE', ( #764, #2920, #7495, #1841 ) ) ;
#12602 = DIRECTION ( 'NONE',  ( 0.000000000000000000, 0.000000000000000000, 1.000000000000000000 ) ) ;
#12603 = CARTESIAN_POINT ( 'NONE',  ( 3.940811704950003325, 32.97290950744599769, 10.00000000000000000 ) ) ;
#12604 = CARTESIAN_POINT ( 'NONE',  ( -18.99164311995750865, 26.94578616932480486, 56.17493374376507376 ) ) ;
#12605 = FACE_OUTER_BOUND ( 'NONE', #13703, .T. ) ;
#12606 = DIRECTION ( 'NONE',  ( 0.000000000000000000, 0.000000000000000000, 1.000000000000000000 ) ) ;
#12607 = CIRCLE ( 'NONE', #11487, 7.166108729582679970 ) ;
#12608 = DIRECTION ( 'NONE',  ( -0.000000000000000000, -1.000000000000000000, -0.000000000000000000 ) ) ;
#12609 = DIRECTION ( 'NONE',  ( 0.9948896271464819918, 0.1009684594134925978, 0.000000000000000000 ) ) ;
#12610 = ORIENTED_EDGE ( 'NONE', *, *, #9594, .T. ) ;
#12611 = EDGE_CURVE ( 'NONE', #3610, #13231, #9123, .T. ) ;
#12612 = EDGE_CURVE ( 'NONE', #5295, #11937, #646, .T. ) ;
#12613 = EDGE_CURVE ( 'NONE', #2730, #1970, #13522, .T. ) ;
#12614 = VECTOR ( 'NONE', #12425, 1000.000000000000000 ) ;
#12615 = DIRECTION ( 'NONE',  ( -1.000000000000000000, 0.000000000000000000, 0.000000000000000000 ) ) ;
#12616 = VERTEX_POINT ( 'NONE', #2159 ) ;
#12617 = ORIENTED_EDGE ( 'NONE', *, *, #1060, .F. ) ;
#12618 = CARTESIAN_POINT ( 'NONE',  ( -24.20502162805000168, 10.97290950744599947, 60.60999999999999943 ) ) ;
#12619 = DIRECTION ( 'NONE',  ( -0.000000000000000000, -1.000000000000000000, -0.000000000000000000 ) ) ;
#12620 = FACE_OUTER_BOUND ( 'NONE', #2134, .T. ) ;
#12621 = CYLINDRICAL_SURFACE ( 'NONE', #7383, 1.999999999999986233 ) ;
#12622 = VERTEX_POINT ( 'NONE', #7362 ) ;
#12623 = DIRECTION ( 'NONE',  ( 0.000000000000000000, 0.000000000000000000, -1.000000000000000000 ) ) ;
#12624 = CYLINDRICAL_SURFACE ( 'NONE', #11120, 2.000000000000001776 ) ;
#12625 = DIRECTION ( 'NONE',  ( 0.000000000000000000, -1.000000000000000000, 0.000000000000000000 ) ) ;
#12626 = CARTESIAN_POINT ( 'NONE',  ( -18.05918829504999934, 10.97290950744599947, 60.04999999999999716 ) ) ;
#12627 =( NAMED_UNIT ( * ) SI_UNIT ( $, .STERADIAN. ) SOLID_ANGLE_UNIT ( ) );
#12628 = EDGE_CURVE ( 'NONE', #5559, #8370, #3120, .T. ) ;
#12629 = VECTOR ( 'NONE', #4443, 1000.000000000000114 ) ;
#12630 = VERTEX_POINT ( 'NONE', #45 ) ;
#12631 = EDGE_CURVE ( 'NONE', #7318, #4114, #1756, .T. ) ;
#12632 = EDGE_CURVE ( 'NONE', #12239, #5283, #8426, .T. ) ;
#12633 = ORIENTED_EDGE ( 'NONE', *, *, #11225, .F. ) ;
#12634 = DIRECTION ( 'NONE',  ( 1.000000000000000000, 0.000000000000000000, 0.000000000000000000 ) ) ;
#12635 = VERTEX_POINT ( 'NONE', #6396 ) ;
#12636 = ORIENTED_EDGE ( 'NONE', *, *, #7403, .T. ) ;
#12637 = ORIENTED_EDGE ( 'NONE', *, *, #12780, .T. ) ;
#12638 = DIRECTION ( 'NONE',  ( 0.000000000000000000, 0.000000000000000000, -1.000000000000000000 ) ) ;
#12639 = ORIENTED_EDGE ( 'NONE', *, *, #2598, .F. ) ;
#12640 = VECTOR ( 'NONE', #3035, 1000.000000000000114 ) ;
#12641 = CARTESIAN_POINT ( 'NONE',  ( -35.05918829505000645, 27.97290950744599769, 0.000000000000000000 ) ) ;
#12642 = DIRECTION ( 'NONE',  ( 1.000000000000000000, 0.000000000000000000, 0.000000000000000000 ) ) ;
#12643 = CARTESIAN_POINT ( 'NONE',  ( 134.7391892930474739, 108.8019446284309737, 23.00000000000000000 ) ) ;
#12644 = CARTESIAN_POINT ( 'NONE',  ( 134.6356359024541973, 94.90549801902423610, 22.89644660940672694 ) ) ;
#12645 = CIRCLE ( 'NONE', #4178, 4.750000000000000888 ) ;
#12646 = EDGE_CURVE ( 'NONE', #2414, #8660, #9564, .T. ) ;
#12647 = CARTESIAN_POINT ( 'NONE',  ( -14.58337460918420980, 30.09884447278222197, 55.52393896758509584 ) ) ;
#12648 = ORIENTED_EDGE ( 'NONE', *, *, #2968, .T. ) ;
#12649 = VERTEX_POINT ( 'NONE', #10662 ) ;
#12650 = ORIENTED_EDGE ( 'NONE', *, *, #6812, .T. ) ;
#12651 = CYLINDRICAL_SURFACE ( 'NONE', #7939, 0.2500000000000002220 ) ;
#12652 = FILL_AREA_STYLE_COLOUR ( '', #284 ) ;
#12653 = CLOSED_SHELL ( 'NONE', ( #1526, #12011, #13283, #7751, #3290, #10985, #6544, #7453, #5654, #5454, #10551, #8964, #11603, #11814, #10880, #406, #7047, #10381, #3230 ) ) ;
#12654 = CARTESIAN_POINT ( 'NONE',  ( -34.72201093190195564, 10.97290950744599947, 6.250000000000000000 ) ) ;
#12655 = ORIENTED_EDGE ( 'NONE', *, *, #5883, .T. ) ;
#12656 = CARTESIAN_POINT ( 'NONE',  ( 20.45469220996244175, 1.832421873814834123, 7.000000000000000000 ) ) ;
#12657 = DIRECTION ( 'NONE',  ( 0.000000000000000000, 0.000000000000000000, 1.000000000000000000 ) ) ;
#12658 = AXIS2_PLACEMENT_3D ( 'NONE', #11785, #1234, #1031 ) ;
#12659 = CARTESIAN_POINT ( 'NONE',  ( -28.87730642030695094, 29.81324547859994922, 17.25000000000000000 ) ) ;
#12660 = CARTESIAN_POINT ( 'NONE',  ( -17.86151640326295365, 27.97292178005357499, 58.85016477904981258 ) ) ;
#12661 = CARTESIAN_POINT ( 'NONE',  ( 142.6356359024541973, 85.03908161011133870, 0.7500000000000006661 ) ) ;
#12662 = VECTOR ( 'NONE', #9467, 1000.000000000000000 ) ;
#12663 = ORIENTED_EDGE ( 'NONE', *, *, #7629, .T. ) ;
#12664 = ORIENTED_EDGE ( 'NONE', *, *, #5332, .F. ) ;
#12665 = EDGE_LOOP ( 'NONE', ( #377, #11862, #2295, #1765 ) ) ;
#12666 = EDGE_CURVE ( 'NONE', #3713, #4189, #8001, .T. ) ;
#12667 = CARTESIAN_POINT ( 'NONE',  ( -40.05918829505000645, 35.97290950744599058, 10.00000000000000000 ) ) ;
#12668 = ADVANCED_FACE ( 'NONE', ( #2093 ), #6541, .F. ) ;
#12669 = DIRECTION ( 'NONE',  ( 1.000000000000000000, 0.000000000000000000, 0.000000000000000000 ) ) ;
#12670 = EDGE_LOOP ( 'NONE', ( #11275, #8697, #10168, #11926 ) ) ;
#12671 = CARTESIAN_POINT ( 'NONE',  ( 44.88563590245420443, 94.65549801902425031, 23.00000000000000000 ) ) ;
#12672 = CONICAL_SURFACE ( 'NONE', #11561, 6.850000000000002309, 0.7853981633974433940 ) ;
#12673 = CARTESIAN_POINT ( 'NONE',  ( -18.33386804087177779, 26.97094072739188064, 55.86735471292099930 ) ) ;
#12674 = AXIS2_PLACEMENT_3D ( 'NONE', #1435, #3619, #385 ) ;
#12675 = DIRECTION ( 'NONE',  ( 0.000000000000000000, -1.000000000000000000, 0.000000000000000000 ) ) ;
#12676 = DIRECTION ( 'NONE',  ( -1.000000000000000000, 0.000000000000000000, 0.000000000000000000 ) ) ;
#12677 = VECTOR ( 'NONE', #1419, 1000.000000000000000 ) ;
#12678 = DIRECTION ( 'NONE',  ( 1.000000000000000000, 0.000000000000000000, 0.000000000000000000 ) ) ;
#12679 = ITEM_DEFINED_TRANSFORMATION ( 'NONE', 'NONE', #10251,  #6434 ) ;
#12680 = COLOUR_RGB ( '', 0.66274510, 0.83137255, 0.94901961) ;
#12681 = AXIS2_PLACEMENT_3D ( 'NONE', #12212, #11099, #12075 ) ;
#12682 = ORIENTED_EDGE ( 'NONE', *, *, #12222, .T. ) ;
#12683 = CARTESIAN_POINT ( 'NONE',  ( -18.05918829504999934, 10.97290950744599947, 14.00000000000000000 ) ) ;
#12684 = DIRECTION ( 'NONE',  ( -0.000000000000000000, -0.000000000000000000, 1.000000000000000000 ) ) ;
#12685 = ORIENTED_EDGE ( 'NONE', *, *, #8612, .F. ) ;
#12686 = DIRECTION ( 'NONE',  ( -1.000000000000000000, 0.000000000000000000, 0.000000000000000000 ) ) ;
#12687 = EDGE_CURVE ( 'NONE', #6660, #3775, #3730, .T. ) ;
#12688 = CARTESIAN_POINT ( 'NONE',  ( -18.05918829504999934, 10.97290950744599947, 57.35000000000000142 ) ) ;
#12689 = DIRECTION ( 'NONE',  ( 0.000000000000000000, 0.000000000000000000, -1.000000000000000000 ) ) ;
#12690 = DIRECTION ( 'NONE',  ( 0.000000000000000000, 0.000000000000000000, -1.000000000000000000 ) ) ;
#12691 = VERTEX_POINT ( 'NONE', #7562 ) ;
#12692 = CARTESIAN_POINT ( 'NONE',  ( 44.73918929304747394, 104.0090514096174843, 23.00000000000000000 ) ) ;
#12693 = EDGE_CURVE ( 'NONE', #13362, #3609, #3552, .T. ) ;
#12694 = CARTESIAN_POINT ( 'NONE',  ( -10.81426999815532852, 15.06602133594271820, -3.000000000000000000 ) ) ;
#12695 = DIRECTION ( 'NONE',  ( -0.9496839325805410681, 0.3132098788326420080, 0.000000000000000000 ) ) ;
#12696 = EDGE_CURVE ( 'NONE', #10605, #3613, #8625, .T. ) ;
#12697 = FACE_OUTER_BOUND ( 'NONE', #1474, .T. ) ;
#12698 = PRODUCT_DEFINITION_FORMATION_WITH_SPECIFIED_SOURCE ( 'ANY', '', #9660, .NOT_KNOWN. ) ;
#12699 = VECTOR ( 'NONE', #8589, 1000.000000000000000 ) ;
#12700 = ORIENTED_EDGE ( 'NONE', *, *, #10117, .T. ) ;
#12701 = LINE ( 'NONE', #8504, #8155 ) ;
#12702 = VERTEX_POINT ( 'NONE', #12887 ) ;
#12703 = ORIENTED_EDGE ( 'NONE', *, *, #3714, .F. ) ;
#12704 = ADVANCED_FACE ( 'NONE', ( #11853 ), #2304, .T. ) ;
#12705 = LINE ( 'NONE', #13738, #1945 ) ;
#12706 = CARTESIAN_POINT ( 'NONE',  ( -1.336558817843898073, 10.00028003023991907, 62.14999999999999858 ) ) ;
#12707 = AXIS2_PLACEMENT_3D ( 'NONE', #4980, #13432, #925 ) ;
#12708 = DIRECTION ( 'NONE',  ( -0.000000000000000000, 1.000000000000000000, -0.000000000000000000 ) ) ;
#12709 = CARTESIAN_POINT ( 'NONE',  ( -15.94576320551015236, 6.169660524810645086, 68.60247846904903213 ) ) ;
#12710 = CIRCLE ( 'NONE', #10934, 2.700000000000001066 ) ;
#12711 = DIRECTION ( 'NONE',  ( -1.000000000000000000, 0.000000000000000000, 0.000000000000000000 ) ) ;
#12712 = EDGE_CURVE ( 'NONE', #7844, #13212, #2003, .T. ) ;
#12713 = AXIS2_PLACEMENT_3D ( 'NONE', #12023, #4762, #4554 ) ;
#12714 = AXIS2_PLACEMENT_3D ( 'NONE', #4160, #8409, #12678 ) ;
#12715 = ORIENTED_EDGE ( 'NONE', *, *, #8899, .F. ) ;
#12716 = B_SPLINE_CURVE_WITH_KNOTS ( 'NONE', 3,
 ( #7894, #12169, #11263, #12379, #4626, #1550, #1685, #5926, #6918, #2620, #8886, #12237, #2693, #3589, #10086, #9023, #508, #7826, #6846, #11124, #13276, #11192, #10215, #635, #13419, #3864, #8114, #6721, #1972, #1835, #9236, #13686, #6073, #1760, #11462, #6004, #3033, #2970, #13486, #6212, #4970, #9501, #10288, #4132, #700, #3927, #7185, #8317, #10409, #7246, #8383, #8174, #12438, #7316, #10555, #10482, #5102, #1898, #910, #2898, #13746, #13618, #6138, #9441, #11600, #7117, #7050, #4073, #984, #8450, #11525, #12510, #12582, #834, #773, #5171, #11394, #9370, #12647, #3094, #2051, #6294, #5233, #4201, #13547, #2827, #11324, #10348, #5030, #9300, #3999, #8247, #9781, #6418, #12782, #4476, #3362, #12838, #11673, #8731, #6354, #10829, #131, #5499, #10691, #4276, #6625, #2181, #8581, #1321, #8519, #3233, #1247, #11881, #2258, #12717, #12913, #10763, #9711, #5435, #204, #8648, #1107, #1180, #7593, #2334, #7442, #4401, #10619, #12989, #3437, #7663, #5575, #11946, #4548, #6496, #9865, #6561, #2400, #10901, #288 ),
 .UNSPECIFIED., .F., .F.,
 ( 4, 2, 1, 1, 2, 2, 2, 2, 1, 1, 2, 2, 2, 2, 1, 1, 1, 2, 2, 2, 2, 2, 2, 2, 1, 1, 2, 2, 2, 2, 1, 1, 2, 2, 2, 2, 1, 2, 2, 2, 2, 2, 1, 1, 2, 2, 2, 2, 1, 1, 2, 2, 2, 2, 1, 1, 1, 1, 2, 2, 2, 2, 1, 1, 2, 2, 2, 2, 1, 1, 2, 2, 2, 2, 1, 1, 2, 2, 2, 2, 1, 2, 2, 4 ),
 ( 0.000000000000000000, 0.03125000000000808381, 0.04687500000001171285, 0.05468750000001329492, 0.05859375000001391248, 0.06250000000001453004, 0.09375000000002493838, 0.1093750000000304895, 0.1171875000000335981, 0.1210937500000347916, 0.1230468750000347222, 0.1250000000000346390, 0.1562500000000229816, 0.1718750000000167089, 0.1796875000000135725, 0.1835937500000119627, 0.1855468750000118794, 0.1865234375000117961, 0.1875000000000117129, 0.2031250000000025535, 0.2109374999999971134, 0.2187499999999916733, 0.2343749999999801548, 0.2421874999999742706, 0.2460937499999713562, 0.2480468749999690525, 0.2490234374999678868, 0.2499999999999667211, 0.2812499999999455436, 0.2968749999999342193, 0.3046874999999286127, 0.3085937499999257261, 0.3105468749999242828, 0.3124999999999228395, 0.3437499999998901434, 0.3593749999998738787, 0.3671874999998657740, 0.3710937499998609446, 0.3749999999998561151, 0.4999999999997231659, 0.5624999999996567190, 0.5937499999996241895, 0.6093749999996073141, 0.6171874999995996536, 0.6210937499995951017, 0.6249999999995905497, 0.6562499999995563549, 0.6718749999995385913, 0.6796874999995304867, 0.6835937499995262678, 0.6855468749995233813, 0.6874999999995206057, 0.7187499999994910738, 0.7343749999994761968, 0.7421874999994693134, 0.7460937499994665378, 0.7480468749994652056, 0.7490234374994638733, 0.7495117187494632072, 0.7499999999994625410, 0.7656249999995053956, 0.7734374999995261568, 0.7773437499995370370, 0.7792968749995425881, 0.7802734374995453637, 0.7812499999995481392, 0.7968749999995949906, 0.8046874999996184163, 0.8085937499996297406, 0.8105468749996348476, 0.8115234374996367350, 0.8124999999996386224, 0.8437499999997121192, 0.8593749999997484235, 0.8671874999997662981, 0.8710937499997747357, 0.8730468749997783995, 0.8749999999997821742, 0.9062499999998400169, 0.9218749999998684386, 0.9296874999998825384, 0.9335937499998891997, 0.9374999999998958611, 1.000000000000000000 ),
 .UNSPECIFIED. ) ;
#12717 = CARTESIAN_POINT ( 'NONE',  ( -15.82084781710581289, 30.25218297716627092, 53.82068884647250684 ) ) ;
#12718 = ORIENTED_EDGE ( 'NONE', *, *, #8159, .T. ) ;
#12719 = ORIENTED_EDGE ( 'NONE', *, *, #6770, .F. ) ;
#12721 = ORIENTED_EDGE ( 'NONE', *, *, #7155, .T. ) ;
#12720 = EDGE_CURVE ( 'NONE', #13004, #7458, #3411, .T. ) ;
#12722 = DIRECTION ( 'NONE',  ( -1.000000000000000000, 0.000000000000000000, 0.000000000000000000 ) ) ;
#12723 = CARTESIAN_POINT ( 'NONE',  ( -10.38347696868452097, 26.08535324214045303, 60.85000000000000142 ) ) ;
#12724 = CARTESIAN_POINT ( 'NONE',  ( -40.05918829505000645, 35.97290950744599769, 10.00000000000000000 ) ) ;
#12725 = DIRECTION ( 'NONE',  ( 0.000000000000000000, 0.000000000000000000, 1.000000000000000000 ) ) ;
#12726 = CARTESIAN_POINT ( 'NONE',  ( 2.262399129208274129, 22.44393519180576746, 83.57661607529820458 ) ) ;
#12727 = AXIS2_PLACEMENT_3D ( 'NONE', #12758, #1935, #10529 ) ;
#12728 = AXIS2_PLACEMENT_3D ( 'NONE', #3707, #11314, #7884 ) ;
#12729 = AXIS2_PLACEMENT_3D ( 'NONE', #3375, #9934, #10993 ) ;
#12730 = VECTOR ( 'NONE', #10755, 1000.000000000000000 ) ;
#12731 = CARTESIAN_POINT ( 'NONE',  ( 0.09777679598749940137, 23.36596564213564875, 64.85000000000000853 ) ) ;
#12732 = EDGE_CURVE ( 'NONE', #1952, #5721, #4664, .T. ) ;
#12733 = FACE_OUTER_BOUND ( 'NONE', #1769, .T. ) ;
#12734 = ORIENTED_EDGE ( 'NONE', *, *, #12496, .F. ) ;
#12735 = EDGE_LOOP ( 'NONE', ( #5044, #9066 ) ) ;
#12736 = AXIS2_PLACEMENT_3D ( 'NONE', #12355, #339, #13187 ) ;
#12737 = AXIS2_PLACEMENT_3D ( 'NONE', #4047, #12562, #8497 ) ;
#12738 = VERTEX_POINT ( 'NONE', #4176 ) ;
#12739 = ORIENTED_EDGE ( 'NONE', *, *, #2631, .F. ) ;
#12740 = ORIENTED_EDGE ( 'NONE', *, *, #6002, .T. ) ;
#12741 = DIRECTION ( 'NONE',  ( 0.000000000000000000, 0.000000000000000000, 1.000000000000000000 ) ) ;
#12742 = DIRECTION ( 'NONE',  ( 0.000000000000000000, 0.000000000000000000, 1.000000000000000000 ) ) ;
#12743 = ORIENTED_EDGE ( 'NONE', *, *, #1696, .T. ) ;
#12744 = CARTESIAN_POINT ( 'NONE',  ( -36.21615338608749823, -1.420146627243662030, 68.85549045786049760 ) ) ;
#12745 = FACE_OUTER_BOUND ( 'NONE', #9245, .T. ) ;
#12746 = DIRECTION ( 'NONE',  ( 0.000000000000000000, 0.000000000000000000, 1.000000000000000000 ) ) ;
#12747 = LINE ( 'NONE', #8547, #1145 ) ;
#12748 = DIRECTION ( 'NONE',  ( 0.3132098788326400096, -0.9496839325805418452, 0.000000000000000000 ) ) ;
#12749 = AXIS2_PLACEMENT_3D ( 'NONE', #11679, #2121, #11736 ) ;
#12750 =( BOUNDED_SURFACE ( )  B_SPLINE_SURFACE ( 3, 3, ( 
 ( #9736, #10142, #7953, #6910 ),
 ( #1677, #10079, #626, #9157 ),
 ( #237, #6584, #10859, #2820 ),
 ( #5922, #2427, #8684, #1749 ) ),
 .UNSPECIFIED., .F., .F., .F. ) 
 B_SPLINE_SURFACE_WITH_KNOTS ( ( 4, 4 ),
 ( 4, 4 ),
 ( 0.000000000000000000, 1.000000000000000000 ),
 ( 0.000000000000000000, 1.000000000000000000 ),
 .UNSPECIFIED. ) 
 GEOMETRIC_REPRESENTATION_ITEM ( )  RATIONAL_B_SPLINE_SURFACE ( (
 ( 1.000000000000000000, 0.3333333333333329818, 0.3333333333333329818, 1.000000000000000000),
 ( 0.7553208711179729695, 0.2517736237059909898, 0.2517736237059909898, 0.7553208711179729695),
 ( 0.7553208711179729695, 0.2517736237059909898, 0.2517736237059909898, 0.7553208711179729695),
 ( 1.000000000000000000, 0.3333333333333329818, 0.3333333333333329818, 1.000000000000000000) ) ) 
 REPRESENTATION_ITEM ( '' )  SURFACE ( )  );
#12751 = AXIS2_PLACEMENT_3D ( 'NONE', #12603, #2008, #726 ) ;
#12752 = ITEM_DEFINED_TRANSFORMATION ( 'NONE', 'NONE', #3118,  #6434 ) ;
#12753 = EDGE_CURVE ( 'NONE', #2257, #2380, #11714, .T. ) ;
#12754 = ORIENTED_EDGE ( 'NONE', *, *, #80, .F. ) ;
#12755 = AXIS2_PLACEMENT_3D ( 'NONE', #6892, #4744, #11160 ) ;
#12756 = DIRECTION ( 'NONE',  ( 0.7091883091770476710, -0.7050191076322684935, 0.000000000000000000 ) ) ;
#12757 = FACE_BOUND ( 'NONE', #246, .T. ) ;
#12758 = CARTESIAN_POINT ( 'NONE',  ( -1.059188295049996231, -6.027090492554000534, 7.250000000000000000 ) ) ;
#12759 = CARTESIAN_POINT ( 'NONE',  ( -20.31679026759186613, 30.25033400041233733, 53.83638459472079774 ) ) ;
#12760 = FACE_OUTER_BOUND ( 'NONE', #6136, .T. ) ;
#12761 = DIRECTION ( 'NONE',  ( -1.000000000000000000, 0.000000000000000000, 0.000000000000000000 ) ) ;
#12762 = CARTESIAN_POINT ( 'NONE',  ( -22.02876472382295248, 15.47207198241065029, 31.09999999999999787 ) ) ;
#12763 = CARTESIAN_POINT ( 'NONE',  ( 140.6356359024541973, 85.03908161011132449, 19.68933982822018081 ) ) ;
#12764 = ORIENTED_EDGE ( 'NONE', *, *, #13528, .T. ) ;
#12765 = DIRECTION ( 'NONE',  ( 0.000000000000000000, 0.000000000000000000, -1.000000000000000000 ) ) ;
#12766 = CIRCLE ( 'NONE', #4301, 0.5000000000000004441 ) ;
#12767 = EDGE_CURVE ( 'NONE', #9970, #8747, #6339, .T. ) ;
#12768 = EDGE_LOOP ( 'NONE', ( #13535, #13092, #10682, #1414 ) ) ;
#12769 = VERTEX_POINT ( 'NONE', #8496 ) ;
#12770 = EDGE_LOOP ( 'NONE', ( #371, #2622, #449, #9596 ) ) ;
#12771 = LINE ( 'NONE', #9697, #5676 ) ;
#12772 = ORIENTED_EDGE ( 'NONE', *, *, #13444, .T. ) ;
#12773 = VERTEX_POINT ( 'NONE', #12762 ) ;
#12774 = CARTESIAN_POINT ( 'NONE',  ( -13.41866240927501508, 8.399302110258624054, 68.54361232608823684 ) ) ;
#12775 = AXIS2_PLACEMENT_3D ( 'NONE', #11423, #3742, #11219 ) ;
#12776 = LINE ( 'NONE', #6484, #9616 ) ;
#12777 = DIRECTION ( 'NONE',  ( 0.7071067811865489050, 0.000000000000000000, -0.7071067811865460184 ) ) ;
#12778 = CARTESIAN_POINT ( 'NONE',  ( 92.63563590245421153, 112.2890816101113387, 19.25000000000000000 ) ) ;
#12779 = CARTESIAN_POINT ( 'NONE',  ( 68.49370948373500312, 85.03908161011133870, 0.7500000000000006661 ) ) ;
#12780 = EDGE_CURVE ( 'NONE', #1687, #10704, #3209, .T. ) ;
#12781 = AXIS2_PLACEMENT_3D ( 'NONE', #11408, #9032, #12248 ) ;
#12782 = CARTESIAN_POINT ( 'NONE',  ( -15.25210833619480510, 30.19004818236263077, 54.39484650223464257 ) ) ;
#12783 = ORIENTED_EDGE ( 'NONE', *, *, #1611, .T. ) ;
#12784 = ORIENTED_EDGE ( 'NONE', *, *, #770, .F. ) ;
#12785 = CARTESIAN_POINT ( 'NONE',  ( -18.05918829504999934, 10.97290950744599947, 68.84999999999999432 ) ) ;
#12786 = EDGE_CURVE ( 'NONE', #999, #8284, #7781, .T. ) ;
#12787 = DIRECTION ( 'NONE',  ( -1.000000000000000000, 0.000000000000000000, 0.000000000000000000 ) ) ;
#12788 =( NAMED_UNIT ( * ) SI_UNIT ( $, .STERADIAN. ) SOLID_ANGLE_UNIT ( ) );
#12789 = ORIENTED_EDGE ( 'NONE', *, *, #982, .F. ) ;
#12790 = CARTESIAN_POINT ( 'NONE',  ( -18.05918829504999934, 10.97290950744599947, 12.50000000000000000 ) ) ;
#12791 = LINE ( 'NONE', #12726, #4885 ) ;
#12792 = AXIS2_PLACEMENT_3D ( 'NONE', #10195, #1811, #680 ) ;
#12793 = CARTESIAN_POINT ( 'NONE',  ( -18.05918829504999934, 2.892876190446000084, 63.34900083300000517 ) ) ;
#12794 = CARTESIAN_POINT ( 'NONE',  ( -5.631644894983189431, 10.97290950744599947, 73.76763816269230745 ) ) ;
#12795 = ADVANCED_FACE ( 'NONE', ( #7639 ), #9904, .T. ) ;
#12796 = ORIENTED_EDGE ( 'NONE', *, *, #5011, .T. ) ;
#12797 = CYLINDRICAL_SURFACE ( 'NONE', #3248, 4.749999999999997335 ) ;
#12798 = ORIENTED_EDGE ( 'NONE', *, *, #7168, .T. ) ;
#12799 = ORIENTED_EDGE ( 'NONE', *, *, #8761, .T. ) ;
#12800 = ORIENTED_EDGE ( 'NONE', *, *, #8529, .F. ) ;
#12801 = ADVANCED_FACE ( 'NONE', ( #7704 ), #12464, .T. ) ;
#12802 = DIRECTION ( 'NONE',  ( -0.08563346120589268584, -1.048707441657055866E-17, -0.9963267086261908823 ) ) ;
#12803 = CARTESIAN_POINT ( 'NONE',  ( -25.73489962141544751, -4.139534227248430120, 60.85000000000000142 ) ) ;
#12804 = VERTEX_POINT ( 'NONE', #4731 ) ;
#12805 = CARTESIAN_POINT ( 'NONE',  ( -18.05918829504999934, 30.47290950744599769, 57.35000000000000142 ) ) ;
#12806 = DIRECTION ( 'NONE',  ( 0.000000000000000000, 0.000000000000000000, 1.000000000000000000 ) ) ;
#12807 = LINE ( 'NONE', #1138, #1967 ) ;
#12808 = DIRECTION ( 'NONE',  ( 1.000000000000000000, 0.000000000000000000, 0.000000000000000000 ) ) ;
#12809 = CARTESIAN_POINT ( 'NONE',  ( 3.190811704950004657, 27.97290950744599769, 64.35000000000000853 ) ) ;
#12810 = ORIENTED_EDGE ( 'NONE', *, *, #13134, .F. ) ;
#12811 = EDGE_CURVE ( 'NONE', #6784, #999, #11021, .T. ) ;
#12812 = CARTESIAN_POINT ( 'NONE',  ( -38.63164489498320364, 10.97290950744599947, 64.85000000000000853 ) ) ;
#12813 = ORIENTED_EDGE ( 'NONE', *, *, #12580, .T. ) ;
#12814 = EDGE_CURVE ( 'NONE', #3894, #12773, #8986, .T. ) ;
#12815 = DIRECTION ( 'NONE',  ( 0.000000000000000000, 0.000000000000000000, 1.000000000000000000 ) ) ;
#12816 = DIRECTION ( 'NONE',  ( 0.4528443260392608916, 0.8915896008669277339, 0.000000000000000000 ) ) ;
#12817 = CARTESIAN_POINT ( 'NONE',  ( -12.26420230435512160, 9.417873376788568507, 67.84999999999999432 ) ) ;
#12818 = CIRCLE ( 'NONE', #3036, 4.750000000000000000 ) ;
#12819 = DIRECTION ( 'NONE',  ( -0.000000000000000000, -0.000000000000000000, 1.000000000000000000 ) ) ;
#12820 =( BOUNDED_CURVE ( )  B_SPLINE_CURVE ( 3, ( #7126, #6994, #8181, #10354 ),
 .UNSPECIFIED., .F., .T. ) 
 B_SPLINE_CURVE_WITH_KNOTS ( ( 4, 4 ),
 ( 1.570796326794896558, 3.141592653589793560 ),
 .UNSPECIFIED. ) 
 CURVE ( )  GEOMETRIC_REPRESENTATION_ITEM ( )  RATIONAL_B_SPLINE_CURVE ( ( 1.000000000000000000, 0.8047378541243649375, 0.8047378541243649375, 1.000000000000000000 ) ) 
 REPRESENTATION_ITEM ( '' )  );
#12821 = FACE_OUTER_BOUND ( 'NONE', #9461, .T. ) ;
#12822 = DIRECTION ( 'NONE',  ( -1.000000000000000000, 0.000000000000000000, 0.000000000000000000 ) ) ;
#12823 = CARTESIAN_POINT ( 'NONE',  ( -1.059188295049996231, -6.027090492554000534, 5.250000000000000000 ) ) ;
#12824 = FACE_BOUND ( 'NONE', #7835, .T. ) ;
#12825 = DIRECTION ( 'NONE',  ( 0.000000000000000000, 0.000000000000000000, 1.000000000000000000 ) ) ;
#12826 = CIRCLE ( 'NONE', #11494, 1.999999999999995781 ) ;
#12827 = DIRECTION ( 'NONE',  ( 0.9496839325805410681, -0.3132098788326420080, 0.000000000000000000 ) ) ;
#12828 = FACE_OUTER_BOUND ( 'NONE', #7141, .T. ) ;
#12829 = CYLINDRICAL_SURFACE ( 'NONE', #2500, 8.250000000000001776 ) ;
#12830 = ADVANCED_FACE ( 'NONE', ( #8777, #7918 ), #3621, .F. ) ;
#12831 = FACE_OUTER_BOUND ( 'NONE', #12182, .T. ) ;
#12832 = EDGE_CURVE ( 'NONE', #10749, #6706, #12250, .T. ) ;
#12833 = AXIS2_PLACEMENT_3D ( 'NONE', #1508, #6885, #3483 ) ;
#12834 = DIRECTION ( 'NONE',  ( 0.3202092937642119774, 0.6304490528084099044, 0.7071067811865499042 ) ) ;
#12835 = CARTESIAN_POINT ( 'NONE',  ( -18.05918829504999934, 10.97290950744599947, 30.59999999999999787 ) ) ;
#12836 = ORIENTED_EDGE ( 'NONE', *, *, #739, .F. ) ;
#12837 = AXIS2_PLACEMENT_3D ( 'NONE', #10587, #3134, #3328 ) ;
#12838 = CARTESIAN_POINT ( 'NONE',  ( -15.27055863119252699, 30.19228463276535734, 54.37235416479132510 ) ) ;
#12839 = ORIENTED_EDGE ( 'NONE', *, *, #8464, .F. ) ;
#12840 = DIRECTION ( 'NONE',  ( 0.000000000000000000, 0.000000000000000000, 1.000000000000000000 ) ) ;
#12841 = DIRECTION ( 'NONE',  ( 0.9496839325805410681, 0.3132098788326420080, 0.000000000000000000 ) ) ;
#12842 = DIRECTION ( 'NONE',  ( 0.2878798879079283446, -0.9576665234506834823, 0.000000000000000000 ) ) ;
#12843 = ORIENTED_EDGE ( 'NONE', *, *, #6104, .T. ) ;
#12844 = ORIENTED_EDGE ( 'NONE', *, *, #2165, .F. ) ;
#12845 = CARTESIAN_POINT ( 'NONE',  ( 109.6856792294029219, 115.9888905337886769, 20.00000000000000000 ) ) ;
#12846 = DIRECTION ( 'NONE',  ( 0.4528443260392608360, 0.8915896008669278450, 0.000000000000000000 ) ) ;
#12847 = EDGE_CURVE ( 'NONE', #10843, #8732, #3994, .T. ) ;
#12848 = CARTESIAN_POINT ( 'NONE',  ( -18.05918829504999934, 10.00028003023991907, 62.14999999999999858 ) ) ;
#12849 = AXIS2_PLACEMENT_3D ( 'NONE', #4817, #422, #12221 ) ;
#12850 = EDGE_CURVE ( 'NONE', #6180, #2221, #10952, .T. ) ;
#12851 = CARTESIAN_POINT ( 'NONE',  ( -18.05918829504999934, 7.130333642789880244, 68.85549045786049760 ) ) ;
#12852 = EDGE_CURVE ( 'NONE', #9911, #6154, #8896, .T. ) ;
#12853 = EDGE_CURVE ( 'NONE', #8119, #11975, #5760, .T. ) ;
#12854 = ORIENTED_EDGE ( 'NONE', *, *, #2398, .T. ) ;
#12855 = ORIENTED_EDGE ( 'NONE', *, *, #739, .T. ) ;
#12856 = CARTESIAN_POINT ( 'NONE',  ( 27.50000000000001066, 9.000000000000000000, 29.99999999999999645 ) ) ;
#12857 = APPLICATION_CONTEXT ( 'automotive_design' ) ;
#12858 = VERTEX_POINT ( 'NONE', #1372 ) ;
#12859 = ORIENTED_EDGE ( 'NONE', *, *, #13194, .F. ) ;
#12860 = VERTEX_POINT ( 'NONE', #5624 ) ;
#12861 = VECTOR ( 'NONE', #7088, 1000.000000000000000 ) ;
#12862 = EDGE_CURVE ( 'NONE', #2149, #9409, #327, .T. ) ;
#12863 = ORIENTED_EDGE ( 'NONE', *, *, #2712, .F. ) ;
#12864 = CARTESIAN_POINT ( 'NONE',  ( 111.0903281124166710, 100.8715034839261762, 10.00000000000000000 ) ) ;
#12865 = DIRECTION ( 'NONE',  ( 1.000000000000000000, 0.000000000000000000, 0.000000000000000000 ) ) ;
#12866 = EDGE_CURVE ( 'NONE', #11544, #2347, #13170, .T. ) ;
#12867 = VERTEX_POINT ( 'NONE', #8837 ) ;
#12868 = DIRECTION ( 'NONE',  ( -0.000000000000000000, -0.000000000000000000, -1.000000000000000000 ) ) ;
#12869 = DIRECTION ( 'NONE',  ( 0.000000000000000000, 0.000000000000000000, 1.000000000000000000 ) ) ;
#12870 = DIRECTION ( 'NONE',  ( 0.000000000000000000, 0.000000000000000000, 1.000000000000000000 ) ) ;
#12871 = DIRECTION ( 'NONE',  ( 0.000000000000000000, 0.000000000000000000, -1.000000000000000000 ) ) ;
#12872 = EDGE_CURVE ( 'NONE', #8206, #11674, #5736, .T. ) ;
#12873 = CARTESIAN_POINT ( 'NONE',  ( -30.48673169511680214, 10.97290950744599947, 17.25000000000000000 ) ) ;
#12874 = SHAPE_DEFINITION_REPRESENTATION ( #2602, #12309 ) ;
#12875 = AXIS2_PLACEMENT_3D ( 'NONE', #4331, #2388, #9854 ) ;
#12876 = EDGE_CURVE ( 'NONE', #4017, #1393, #5827, .T. ) ;
#12877 = DIRECTION ( 'NONE',  ( -0.6615960714621564875, 0.7498604124941129490, 0.000000000000000000 ) ) ;
#12878 = CIRCLE ( 'NONE', #10216, 4.250000000000003553 ) ;
#12879 = DIRECTION ( 'NONE',  ( 0.000000000000000000, 1.000000000000000000, 0.000000000000000000 ) ) ;
#12880 = AXIS2_PLACEMENT_3D ( 'NONE', #13169, #2528, #10053 ) ;
#12881 = CARTESIAN_POINT ( 'NONE',  ( 74.18094369249178044, 97.20665973629650125, 20.00000000000000000 ) ) ;
#12882 = ADVANCED_FACE ( 'NONE', ( #10875 ), #1505, .T. ) ;
#12883 = CIRCLE ( 'NONE', #7284, 1.999999999999986233 ) ;
#12884 = CARTESIAN_POINT ( 'NONE',  ( -20.83881167003955781, 30.19337278744001196, 54.36146151962581285 ) ) ;
#12885 = CARTESIAN_POINT ( 'NONE',  ( -18.05918829504999934, 10.97290950744599947, 60.75000000000000000 ) ) ;
#12886 = FACE_OUTER_BOUND ( 'NONE', #11866, .T. ) ;
#12887 = CARTESIAN_POINT ( 'NONE',  ( 44.88563590245420443, 90.15549801902423610, 23.00000000000000000 ) ) ;
#12888 = LINE ( 'NONE', #5625, #684 ) ;
#12889 = DIRECTION ( 'NONE',  ( -1.000000000000000000, 0.000000000000000000, 0.000000000000000000 ) ) ;
#12890 = EDGE_CURVE ( 'NONE', #3252, #12241, #5950, .T. ) ;
#12891 = CIRCLE ( 'NONE', #9782, 34.70000000000000284 ) ;
#12892 = CIRCLE ( 'NONE', #10007, 17.66282263685195275 ) ;
#12893 = LINE ( 'NONE', #7492, #11718 ) ;
#12894 = ORIENTED_EDGE ( 'NONE', *, *, #3008, .T. ) ;
#12895 = ORIENTED_EDGE ( 'NONE', *, *, #12598, .T. ) ;
#12896 = EDGE_LOOP ( 'NONE', ( #9882, #8709, #1581, #894, #3892, #6369 ) ) ;
#12897 = VERTEX_POINT ( 'NONE', #594 ) ;
#12898 = LINE ( 'NONE', #11870, #7730 ) ;
#12899 = CARTESIAN_POINT ( 'NONE',  ( -18.05918829504999934, 10.97290950744599947, 62.14999999999999858 ) ) ;
#12900 = DIRECTION ( 'NONE',  ( 0.000000000000000000, -1.000000000000000000, 0.000000000000000000 ) ) ;
#12901 = CIRCLE ( 'NONE', #5538, 2.000000000000001776 ) ;
#12902 = VECTOR ( 'NONE', #6807, 1000.000000000000000 ) ;
#12903 = LINE ( 'NONE', #9771, #179 ) ;
#12904 = DIRECTION ( 'NONE',  ( 1.000000000000000000, 0.000000000000000000, 0.000000000000000000 ) ) ;
#12905 = VECTOR ( 'NONE', #8047, 1000.000000000000000 ) ;
#12906 = CARTESIAN_POINT ( 'NONE',  ( -27.49999999999998934, 9.000000000000000000, 29.99999999999999645 ) ) ;
#12907 = FACE_OUTER_BOUND ( 'NONE', #2897, .T. ) ;
#12908 = EDGE_CURVE ( 'NONE', #6318, #9883, #12267, .T. ) ;
#12909 = PRODUCT_DEFINITION_FORMATION_WITH_SPECIFIED_SOURCE ( 'ANY', '', #2255, .NOT_KNOWN. ) ;
#12910 = VERTEX_POINT ( 'NONE', #13445 ) ;
#12911 = EDGE_CURVE ( 'NONE', #2972, #363, #8200, .T. ) ;
#12912 = VECTOR ( 'NONE', #10422, 1000.000000000000000 ) ;
#12913 = CARTESIAN_POINT ( 'NONE',  ( -15.82870473472232753, 30.25294134154687598, 53.81423550378804066 ) ) ;
#12914 = DIRECTION ( 'NONE',  ( -0.3132098788326420635, 0.9496839325805410681, 0.000000000000000000 ) ) ;
#12915 = CARTESIAN_POINT ( 'NONE',  ( -6.000000000000000888, 11.99999999999999822, 7.000000000000000000 ) ) ;
#12916 = CARTESIAN_POINT ( 'NONE',  ( -15.54512322349380149, 8.123439939968370993, 27.09999999999999787 ) ) ;
#12917 = ORIENTED_EDGE ( 'NONE', *, *, #2930, .T. ) ;
#12918 = CARTESIAN_POINT ( 'NONE',  ( 42.63563590245419732, 113.0390816101113387, 0.7500000000000006661 ) ) ;
#12919 = LINE ( 'NONE', #4876, #5533 ) ;
#12920 = FACE_OUTER_BOUND ( 'NONE', #3913, .T. ) ;
#12921 = CARTESIAN_POINT ( 'NONE',  ( 111.0903281124166710, 100.8715034839261762, 10.00000000000000000 ) ) ;
#12922 = AXIS2_PLACEMENT_3D ( 'NONE', #5441, #2062, #2273 ) ;
#12923 = CIRCLE ( 'NONE', #11150, 10.74999999999999645 ) ;
#12924 = VERTEX_POINT ( 'NONE', #6097 ) ;
#12925 = ORIENTED_EDGE ( 'NONE', *, *, #2306, .F. ) ;
#12926 = ADVANCED_FACE ( 'NONE', ( #9117 ), #795, .F. ) ;
#12927 = ORIENTED_EDGE ( 'NONE', *, *, #13319, .T. ) ;
#12928 = VERTEX_POINT ( 'NONE', #2925 ) ;
#12929 = CARTESIAN_POINT ( 'NONE',  ( 62.16596598834446752, 129.5087515242215090, 19.25000000000000000 ) ) ;
#12930 = ORIENTED_EDGE ( 'NONE', *, *, #5640, .T. ) ;
#12931 = EDGE_LOOP ( 'NONE', ( #11892, #13733, #11623, #59 ) ) ;
#12932 = ORIENTED_EDGE ( 'NONE', *, *, #11594, .T. ) ;
#12933 = B_SPLINE_CURVE_WITH_KNOTS ( 'NONE', 3,
 ( #6051, #11436, #11368, #9056, #9273, #1875, #10384, #1725, #13315, #8011, #12285, #2736, #2867 ),
 .UNSPECIFIED., .F., .F.,
 ( 4, 1, 1, 1, 1, 1, 2, 2, 4 ),
 ( 0.000000000000000000, 0.2499999999999435452, 0.3749999999999139022, 0.4374999999999008016, 0.4687499999998942513, 0.4843749999998905875, 0.4921874999998887001, 0.4999999999998868128, 1.000000000000000000 ),
 .UNSPECIFIED. ) ;
#12934 = CIRCLE ( 'NONE', #2047, 2.000000000000001776 ) ;
#12935 = PRODUCT ( 'compact pneumatic cylinder', 'compact pneumatic cylinder', '', ( #1143 ) ) ;
#12936 = VECTOR ( 'NONE', #4478, 1000.000000000000000 ) ;
#12937 = DIRECTION ( 'NONE',  ( 0.000000000000000000, 0.000000000000000000, -1.000000000000000000 ) ) ;
#12938 = CARTESIAN_POINT ( 'NONE',  ( -18.05918829504999934, 30.47290950744599769, 52.80340000000000344 ) ) ;
#12939 = PRODUCT_DEFINITION ( 'UNKNOWN', '', #12698, #5012 ) ;
#12940 = DIRECTION ( 'NONE',  ( -0.000000000000000000, -0.000000000000000000, -1.000000000000000000 ) ) ;
#12941 = CARTESIAN_POINT ( 'NONE',  ( 44.63563590245422574, 113.0390816101113387, 19.25000000000000000 ) ) ;
#12942 = EDGE_CURVE ( 'NONE', #4724, #4825, #6861, .T. ) ;
#12943 = CARTESIAN_POINT ( 'NONE',  ( 109.1537879975201406, 82.61803701715820125, 19.25000000000000000 ) ) ;
#12944 = DIRECTION ( 'NONE',  ( 0.4528443260392610026, 0.8915896008669277339, 0.000000000000000000 ) ) ;
#12945 = CYLINDRICAL_SURFACE ( 'NONE', #13604, 3.000000000000002665 ) ;
#12946 = APPLICATION_PROTOCOL_DEFINITION ( 'draft international standard', 'automotive_design', 1998, #3782 ) ;
#12947 = VECTOR ( 'NONE', #10975, 1000.000000000000000 ) ;
#12948 = VECTOR ( 'NONE', #6019, 1000.000000000000000 ) ;
#12949 = CIRCLE ( 'NONE', #6026, 2.700000000000001066 ) ;
#12950 = ADVANCED_FACE ( 'NONE', ( #13577, #1924 ), #13371, .F. ) ;
#12951 = EDGE_LOOP ( 'NONE', ( #8470, #8635, #10851, #3734 ) ) ;
#12952 = CARTESIAN_POINT ( 'NONE',  ( -23.42001676333060090, -4.028726038184999858, 62.14999999999999858 ) ) ;
#12953 = CARTESIAN_POINT ( 'NONE',  ( 8.000000000000001776, 2.000000000000000000, -65.00000000000000000 ) ) ;
#12954 = ORIENTED_EDGE ( 'NONE', *, *, #3018, .F. ) ;
#12955 = DIRECTION ( 'NONE',  ( -0.000000000000000000, -0.000000000000000000, -1.000000000000000000 ) ) ;
#12956 = CARTESIAN_POINT ( 'NONE',  ( 50.63563590245420443, 108.9054980190242503, 22.75000000000000000 ) ) ;
#12957 = EDGE_CURVE ( 'NONE', #13546, #12858, #6186, .T. ) ;
#12958 = CARTESIAN_POINT ( 'NONE',  ( -18.62368403728828170, 30.35356550733773418, 53.03788860485584422 ) ) ;
#12959 = VECTOR ( 'NONE', #12242, 1000.000000000000000 ) ;
#12960 = CIRCLE ( 'NONE', #6935, 6.449999999999997513 ) ;
#12961 = CARTESIAN_POINT ( 'NONE',  ( -3.743645030049981948, 18.13068114044599710, 61.70038048200006386 ) ) ;
#12962 = VECTOR ( 'NONE', #6267, 1000.000000000000000 ) ;
#12963 = DIRECTION ( 'NONE',  ( -1.000000000000000000, 0.000000000000000000, 0.000000000000000000 ) ) ;
#12964 = CARTESIAN_POINT ( 'NONE',  ( -18.05918829504999934, 10.97290950744599947, 63.45000000000000284 ) ) ;
#12965 = CARTESIAN_POINT ( 'NONE',  ( -18.05918829504999934, 10.97290950744599947, 63.54999999999999716 ) ) ;
#12966 = EDGE_CURVE ( 'NONE', #7434, #4562, #12544, .T. ) ;
#12967 = AXIS2_PLACEMENT_3D ( 'NONE', #7740, #6129, #8377 ) ;
#12968 = AXIS2_PLACEMENT_3D ( 'NONE', #12246, #4714, #9031 ) ;
#12969 = CIRCLE ( 'NONE', #10088, 3.500000000000000888 ) ;
#12970 = EDGE_LOOP ( 'NONE', ( #10108, #9863 ) ) ;
#12971 = DIRECTION ( 'NONE',  ( 1.000000000000000000, 0.000000000000000000, -0.000000000000000000 ) ) ;
#12972 = EDGE_LOOP ( 'NONE', ( #10257, #9604, #10971, #772 ) ) ;
#12973 = ORIENTED_EDGE ( 'NONE', *, *, #5061, .F. ) ;
#12974 = CARTESIAN_POINT ( 'NONE',  ( -7.999999999999996447, -1.701580061351808733E-15, 0.000000000000000000 ) ) ;
#12975 = ORIENTED_EDGE ( 'NONE', *, *, #10700, .T. ) ;
#12976 = DIRECTION ( 'NONE',  ( 1.000000000000000000, 0.000000000000000000, 0.000000000000000000 ) ) ;
#12977 = EDGE_CURVE ( 'NONE', #9491, #2697, #1788, .T. ) ;
#12978 = DIRECTION ( 'NONE',  ( 0.000000000000000000, 0.000000000000000000, 1.000000000000000000 ) ) ;
#12979 = DIRECTION ( 'NONE',  ( 0.000000000000000000, 0.000000000000000000, -1.000000000000000000 ) ) ;
#12980 = DIRECTION ( 'NONE',  ( 0.000000000000000000, 0.000000000000000000, 1.000000000000000000 ) ) ;
#12981 = CARTESIAN_POINT ( 'NONE',  ( 3.690811704950009986, 27.97290950744599769, 64.85000000000000853 ) ) ;
#12982 = CARTESIAN_POINT ( 'NONE',  ( -24.47918829505000105, 10.97290950744599947, 64.85000000000000853 ) ) ;
#12983 = VECTOR ( 'NONE', #7795, 1000.000000000000000 ) ;
#12984 = CARTESIAN_POINT ( 'NONE',  ( -7.640422211807256225, -16.89844320975769776, 0.000000000000000000 ) ) ;
#12985 = DIRECTION ( 'NONE',  ( -1.000000000000000000, 0.000000000000000000, 0.000000000000000000 ) ) ;
#12986 = UNCERTAINTY_MEASURE_WITH_UNIT (LENGTH_MEASURE( 1.000000000000000082E-05 ), #2098, 'distance_accuracy_value', 'NONE');
#12987 = ORIENTED_EDGE ( 'NONE', *, *, #8087, .F. ) ;
#12988 = AXIS2_PLACEMENT_3D ( 'NONE', #11712, #43, #5210 ) ;
#12989 = CARTESIAN_POINT ( 'NONE',  ( -16.63855339399303901, 30.31714196968558284, 53.30236028803027892 ) ) ;
#12990 = ORIENTED_EDGE ( 'NONE', *, *, #4011, .T. ) ;
#12991 = SURFACE_STYLE_USAGE ( .BOTH. , #289 ) ;
#12992 = CARTESIAN_POINT ( 'NONE',  ( -11.70083760351054103, 35.47811937223634970, 5.250000000000000000 ) ) ;
#12993 = EDGE_CURVE ( 'NONE', #3627, #10303, #2718, .T. ) ;
#12994 = VECTOR ( 'NONE', #8117, 1000.000000000000000 ) ;
#12995 = ORIENTED_EDGE ( 'NONE', *, *, #10827, .F. ) ;
#12996 = DIRECTION ( 'NONE',  ( -0.000000000000000000, -1.000000000000000000, -0.000000000000000000 ) ) ;
#12997 = CYLINDRICAL_SURFACE ( 'NONE', #1793, 6.450000000000001066 ) ;
#12998 = EDGE_CURVE ( 'NONE', #6577, #9897, #11484, .T. ) ;
#12999 = CARTESIAN_POINT ( 'NONE',  ( 8.000000000000001776, 2.000000000000000000, -65.00000000000000000 ) ) ;
#13000 = AXIS2_PLACEMENT_3D ( 'NONE', #1859, #13443, #9116 ) ;
#13001 = ORIENTED_EDGE ( 'NONE', *, *, #8517, .T. ) ;
#13002 = ORIENTED_EDGE ( 'NONE', *, *, #1611, .F. ) ;
#13003 = VERTEX_POINT ( 'NONE', #868 ) ;
#13004 = VERTEX_POINT ( 'NONE', #5127 ) ;
#13005 = VERTEX_POINT ( 'NONE', #3816 ) ;
#13006 = EDGE_LOOP ( 'NONE', ( #7481, #3361, #7963, #4059 ) ) ;
#13007 = ORIENTED_EDGE ( 'NONE', *, *, #12452, .T. ) ;
#13008 = EDGE_LOOP ( 'NONE', ( #9583, #12099, #2182, #11559 ) ) ;
#13009 = FACE_OUTER_BOUND ( 'NONE', #10596, .T. ) ;
#13010 = CARTESIAN_POINT ( 'NONE',  ( -15.54654308236029792, 19.85770471824265115, 64.85000000000000853 ) ) ;
#13011 = EDGE_LOOP ( 'NONE', ( #4561, #3021, #5153, #6981 ) ) ;
#13012 = DIRECTION ( 'NONE',  ( -0.000000000000000000, -0.000000000000000000, 1.000000000000000000 ) ) ;
#13013 = DIRECTION ( 'NONE',  ( 0.000000000000000000, 1.000000000000000000, 0.000000000000000000 ) ) ;
#13014 = ADVANCED_FACE ( 'NONE', ( #9401 ), #3744, .F. ) ;
#13015 = FACE_OUTER_BOUND ( 'NONE', #8967, .T. ) ;
#13016 = CARTESIAN_POINT ( 'NONE',  ( -1.059188295049996231, 10.97290950744599947, 57.35000000000000142 ) ) ;
#13017 = EDGE_CURVE ( 'NONE', #7262, #8225, #12439, .T. ) ;
#13018 = CARTESIAN_POINT ( 'NONE',  ( -35.05918829505000645, -6.027090492554000534, 64.35000000000000853 ) ) ;
#13019 = CIRCLE ( 'NONE', #4111, 1.999999999999994893 ) ;
#13020 = ORIENTED_EDGE ( 'NONE', *, *, #9951, .T. ) ;
#13021 = ORIENTED_EDGE ( 'NONE', *, *, #4412, .F. ) ;
#13022 = ORIENTED_EDGE ( 'NONE', *, *, #8850, .F. ) ;
#13023 = CARTESIAN_POINT ( 'NONE',  ( -18.05918829504999934, 10.97290950744599947, 0.000000000000000000 ) ) ;
#13024 = VERTEX_POINT ( 'NONE', #3951 ) ;
#13025 = CYLINDRICAL_SURFACE ( 'NONE', #12295, 4.000000000000000888 ) ;
#13026 = CARTESIAN_POINT ( 'NONE',  ( 4.599650328638321461, 0.000000000000000000, 7.878124499050794149 ) ) ;
#13027 = CARTESIAN_POINT ( 'NONE',  ( -20.04570110035189856, 30.27520963117099839, 53.62886082399810306 ) ) ;
#13028 = CARTESIAN_POINT ( 'NONE',  ( -4.499999999999999112, -1.301042606982605321E-15, -65.00000000000000000 ) ) ;
#13029 = CARTESIAN_POINT ( 'NONE',  ( -16.08092853089235774, 0.000000000000000000, 9.237812082545083570 ) ) ;
#13030 = CARTESIAN_POINT ( 'NONE',  ( -27.15409092487699994, 0.3335619008453594714, 62.14999999999999858 ) ) ;
#13031 = DIRECTION ( 'NONE',  ( 0.000000000000000000, 0.000000000000000000, -1.000000000000000000 ) ) ;
#13032 = ADVANCED_FACE ( 'NONE', ( #9258 ), #7071, .F. ) ;
#13033 = CARTESIAN_POINT ( 'NONE',  ( -35.05918829505000645, 27.97290950744599769, 0.000000000000000000 ) ) ;
#13034 =( NAMED_UNIT ( * ) PLANE_ANGLE_UNIT ( ) SI_UNIT ( $, .RADIAN. ) );
#13035 = ORIENTED_EDGE ( 'NONE', *, *, #10237, .F. ) ;
#13036 = EDGE_CURVE ( 'NONE', #11937, #11963, #657, .T. ) ;
#13037 = EDGE_LOOP ( 'NONE', ( #7710, #6572, #13620, #11414 ) ) ;
#13038 = ORIENTED_EDGE ( 'NONE', *, *, #10248, .T. ) ;
#13039 = ORIENTED_EDGE ( 'NONE', *, *, #3001, .F. ) ;
#13040 = CARTESIAN_POINT ( 'NONE',  ( 44.63563590245420443, 103.9054980190242361, 23.00000000000000000 ) ) ;
#13041 = EDGE_LOOP ( 'NONE', ( #9819, #13075, #8785, #5104 ) ) ;
#13042 = ORIENTED_EDGE ( 'NONE', *, *, #13552, .T. ) ;
#13043 = LINE ( 'NONE', #7651, #3593 ) ;
#13044 = CARTESIAN_POINT ( 'NONE',  ( -12.47577096721731849, 9.231207973652310272, 68.00596099852270982 ) ) ;
#13045 = DIRECTION ( 'NONE',  ( 1.000000000000000000, 0.000000000000000000, 0.000000000000000000 ) ) ;
#13046 = DIRECTION ( 'NONE',  ( -0.000000000000000000, -0.000000000000000000, 1.000000000000000000 ) ) ;
#13047 = LINE ( 'NONE', #12146, #4289 ) ;
#13048 = LINE ( 'NONE', #11162, #13341 ) ;
#13049 = CYLINDRICAL_SURFACE ( 'NONE', #6265, 17.66282263685195275 ) ;
#13050 = ADVANCED_FACE ( 'NONE', ( #9193 ), #3888, .T. ) ;
#13051 = CARTESIAN_POINT ( 'NONE',  ( 10.81426999815522549, -15.06602133594279991, 7.000000000000000000 ) ) ;
#13052 = LINE ( 'NONE', #200, #3312 ) ;
#13053 = CIRCLE ( 'NONE', #7440, 33.00000000000000000 ) ;
#13054 = EDGE_LOOP ( 'NONE', ( #4846, #720 ) ) ;
#13055 = EDGE_CURVE ( 'NONE', #4825, #9584, #2286, .T. ) ;
#13056 = PRODUCT_DEFINITION_SHAPE ( 'NONE', 'NONE',  #13809 ) ;
#13057 = EDGE_LOOP ( 'NONE', ( #5602, #1058, #7263, #8062 ) ) ;
#13058 = FACE_OUTER_BOUND ( 'NONE', #1855, .T. ) ;
#13059 = ORIENTED_EDGE ( 'NONE', *, *, #10181, .T. ) ;
#13060 = CYLINDRICAL_SURFACE ( 'NONE', #587, 17.66282263685195275 ) ;
#13061 = AXIS2_PLACEMENT_3D ( 'NONE', #11173, #6704, #2749 ) ;
#13062 = CYLINDRICAL_SURFACE ( 'NONE', #673, 17.00000000000000000 ) ;
#13063 = CYLINDRICAL_SURFACE ( 'NONE', #8053, 0.7500000000000000000 ) ;
#13064 = CARTESIAN_POINT ( 'NONE',  ( 140.6356359024541973, 89.90549801902423610, 22.75000000000000000 ) ) ;
#13065 = DIRECTION ( 'NONE',  ( -1.821689671877679746E-15, -1.000000000000000000, 2.732534507816519619E-15 ) ) ;
#13066 = PLANE ( 'NONE',  #7541 ) ;
#13067 = ADVANCED_FACE ( 'NONE', ( #945 ), #5457, .T. ) ;
#13068 = ORIENTED_EDGE ( 'NONE', *, *, #3672, .T. ) ;
#13069 = ORIENTED_EDGE ( 'NONE', *, *, #1167, .T. ) ;
#13070 = ORIENTED_EDGE ( 'NONE', *, *, #9831, .F. ) ;
#13071 = EDGE_LOOP ( 'NONE', ( #351, #11346, #12320, #12166 ) ) ;
#13072 = CARTESIAN_POINT ( 'NONE',  ( 3.190811704950004657, 27.97290950744599769, 58.85000000000000142 ) ) ;
#13073 = EDGE_LOOP ( 'NONE', ( #3281, #857, #7280, #4343 ) ) ;
#13074 = ORIENTED_EDGE ( 'NONE', *, *, #3418, .F. ) ;
#13075 = ORIENTED_EDGE ( 'NONE', *, *, #2869, .F. ) ;
#13076 = VERTEX_POINT ( 'NONE', #10789 ) ;
#13077 = CARTESIAN_POINT ( 'NONE',  ( -16.04064420431702942, 0.000000000000000000, -11.30758658292224084 ) ) ;
#13078 = CARTESIAN_POINT ( 'NONE',  ( -20.57325336660620252, 13.82237907492362083, 27.09999999999999787 ) ) ;
#13079 = VERTEX_POINT ( 'NONE', #10718 ) ;
#13080 = CARTESIAN_POINT ( 'NONE',  ( -18.05918829504999934, 10.97290950744599947, 60.40999999999999659 ) ) ;
#13081 = DIRECTION ( 'NONE',  ( 0.000000000000000000, 0.000000000000000000, 1.000000000000000000 ) ) ;
#13082 = LINE ( 'NONE', #3525, #12040 ) ;
#13083 = CARTESIAN_POINT ( 'NONE',  ( 9.640422211807132769, 16.89844320975774750, -3.000000000000000000 ) ) ;
#13084 = ORIENTED_EDGE ( 'NONE', *, *, #5943, .T. ) ;
#13085 = EDGE_CURVE ( 'NONE', #10557, #6848, #7739, .T. ) ;
#13086 = EDGE_LOOP ( 'NONE', ( #6938, #11417, #11029, #12498 ) ) ;
#13087 = ORIENTED_EDGE ( 'NONE', *, *, #12048, .T. ) ;
#13088 = ADVANCED_FACE ( 'NONE', ( #12605 ), #2142, .F. ) ;
#13089 = DIRECTION ( 'NONE',  ( -1.000000000000000000, 8.673617379884027583E-16, 0.000000000000000000 ) ) ;
#13090 = DIRECTION ( 'NONE',  ( -0.000000000000000000, -0.000000000000000000, 1.000000000000000000 ) ) ;
#13091 = ADVANCED_FACE ( 'NONE', ( #11757 ), #2079, .T. ) ;
#13092 = ORIENTED_EDGE ( 'NONE', *, *, #11954, .F. ) ;
#13093 = DIRECTION ( 'NONE',  ( -0.000000000000000000, 0.000000000000000000, 1.000000000000000000 ) ) ;
#13094 = CARTESIAN_POINT ( 'NONE',  ( -20.95080569073241605, 30.17981166141560578, 54.49760474301193369 ) ) ;
#13095 = LINE ( 'NONE', #10949, #6964 ) ;
#13096 = DIRECTION ( 'NONE',  ( 0.000000000000000000, 0.000000000000000000, 1.000000000000000000 ) ) ;
#13097 = CARTESIAN_POINT ( 'NONE',  ( 4.599650328638321461, 8.500000000000001776, 7.878124499050794149 ) ) ;
#13098 = CARTESIAN_POINT ( 'NONE',  ( -18.05918829504999934, 10.97290950744599947, 58.54999999999999716 ) ) ;
#13099 = VECTOR ( 'NONE', #3561, 1000.000000000000000 ) ;
#13100 = DIRECTION ( 'NONE',  ( -1.000000000000000000, 0.000000000000000000, 0.000000000000000000 ) ) ;
#13101 = CIRCLE ( 'NONE', #5992, 4.749999999999997335 ) ;
#13102 = ADVANCED_FACE ( 'NONE', ( #11698 ), #10645, .T. ) ;
#13103 = MECHANICAL_DESIGN_GEOMETRIC_PRESENTATION_REPRESENTATION (  '', ( #11770 ), #11994 ) ;
#13104 = FACE_OUTER_BOUND ( 'NONE', #79, .T. ) ;
#13105 = CYLINDRICAL_SURFACE ( 'NONE', #8705, 16.72262947720610171 ) ;
#13106 = EDGE_LOOP ( 'NONE', ( #3048, #4642, #10776, #4147 ) ) ;
#13107 = ORIENTED_EDGE ( 'NONE', *, *, #7727, .F. ) ;
#13108 = LINE ( 'NONE', #7789, #12505 ) ;
#13109 = EDGE_CURVE ( 'NONE', #3193, #8675, #1053, .T. ) ;
#13110 = CARTESIAN_POINT ( 'NONE',  ( 44.63563590245421864, 85.03908161011133870, 20.00000000000000000 ) ) ;
#13111 = DIRECTION ( 'NONE',  ( 0.000000000000000000, -1.000000000000000000, 0.000000000000000000 ) ) ;
#13112 = FACE_OUTER_BOUND ( 'NONE', #3928, .T. ) ;
#13113 = ORIENTED_EDGE ( 'NONE', *, *, #2992, .F. ) ;
#13114 = DIRECTION ( 'NONE',  ( 0.000000000000000000, 0.000000000000000000, 1.000000000000000000 ) ) ;
#13115 = CARTESIAN_POINT ( 'NONE',  ( 7.500000000000000000, -1.762812401309176307E-15, -65.00000000000000000 ) ) ;
#13116 = DIRECTION ( 'NONE',  ( 0.000000000000000000, 0.000000000000000000, -1.000000000000000000 ) ) ;
#13117 = FACE_OUTER_BOUND ( 'NONE', #937, .T. ) ;
#13118 = VECTOR ( 'NONE', #9141, 1000.000000000000000 ) ;
#13119 = AXIS2_PLACEMENT_3D ( 'NONE', #13186, #7865, #8788 ) ;
#13120 = VECTOR ( 'NONE', #1825, 1000.000000000000114 ) ;
#13121 = VECTOR ( 'NONE', #12669, 1000.000000000000000 ) ;
#13122 = ORIENTED_EDGE ( 'NONE', *, *, #9080, .T. ) ;
#13123 = EDGE_CURVE ( 'NONE', #10749, #10483, #12807, .T. ) ;
#13124 = ORIENTED_EDGE ( 'NONE', *, *, #8428, .F. ) ;
#13125 = CARTESIAN_POINT ( 'NONE',  ( 16.08092853089229024, 4.500000000000000000, -11.23781208254518837 ) ) ;
#13126 = ORIENTED_EDGE ( 'NONE', *, *, #1500, .F. ) ;
#13127 = CIRCLE ( 'NONE', #10239, 1.999999999999994893 ) ;
#13128 = AXIS2_PLACEMENT_3D ( 'NONE', #5272, #10535, #12963 ) ;
#13129 = VERTEX_POINT ( 'NONE', #91 ) ;
#13130 = DIRECTION ( 'NONE',  ( -1.000000000000000000, 0.000000000000000000, 0.000000000000000000 ) ) ;
#13131 = DIRECTION ( 'NONE',  ( -0.7050191076322684935, 0.7091883091770476710, 0.000000000000000000 ) ) ;
#13132 = CARTESIAN_POINT ( 'NONE',  ( -18.05918829504999934, 10.97290950744599947, 30.59999999999999787 ) ) ;
#13133 = DIRECTION ( 'NONE',  ( 0.4678190685372728419, -0.5302313826179317902, 0.7071067811865437980 ) ) ;
#13134 = EDGE_CURVE ( 'NONE', #9649, #4386, #8610, .T. ) ;
#13135 = APPLICATION_CONTEXT ( 'automotive_design' ) ;
#13136 = CARTESIAN_POINT ( 'NONE',  ( -7.640422211807256225, -16.89844320975769776, -3.000000000000000000 ) ) ;
#13137 = DIRECTION ( 'NONE',  ( -0.1353548076753729457, -1.657618319688509444E-17, -0.9907971921837297469 ) ) ;
#13138 = AXIS2_PLACEMENT_3D ( 'NONE', #6631, #11808, #10697 ) ;
#13139 = CIRCLE ( 'NONE', #10897, 2.000000000000001776 ) ;
#13140 = EDGE_CURVE ( 'NONE', #9237, #8057, #6629, .T. ) ;
#13141 = CYLINDRICAL_SURFACE ( 'NONE', #2370, 4.250000000000000000 ) ;
#13142 = ORIENTED_EDGE ( 'NONE', *, *, #7508, .T. ) ;
#13143 = ORIENTED_EDGE ( 'NONE', *, *, #1753, .F. ) ;
#13144 = EDGE_LOOP ( 'NONE', ( #11201, #6636, #1197, #12813, #2350 ) ) ;
#13145 = ORIENTED_EDGE ( 'NONE', *, *, #9772, .T. ) ;
#13146 = ORIENTED_EDGE ( 'NONE', *, *, #12853, .F. ) ;
#13147 = CARTESIAN_POINT ( 'NONE',  ( -1.059188295049996231, -6.027090492554000534, 64.85000000000000853 ) ) ;
#13148 = LINE ( 'NONE', #11130, #8432 ) ;
#13149 = ORIENTED_EDGE ( 'NONE', *, *, #11475, .T. ) ;
#13150 = ADVANCED_FACE ( 'NONE', ( #1068 ), #3315, .F. ) ;
#13151 = DIRECTION ( 'NONE',  ( 0.000000000000000000, -1.000000000000000000, 0.000000000000000000 ) ) ;
#13152 = VECTOR ( 'NONE', #9095, 1000.000000000000000 ) ;
#13153 = DIRECTION ( 'NONE',  ( -0.000000000000000000, 1.000000000000000000, -0.000000000000000000 ) ) ;
#13154 = AXIS2_PLACEMENT_3D ( 'NONE', #10042, #461, #7783 ) ;
#13155 = CARTESIAN_POINT ( 'NONE',  ( 140.3856359024541973, 90.15549801902423610, 23.00000000000000000 ) ) ;
#13156 = CARTESIAN_POINT ( 'NONE',  ( -18.05918829504999934, 10.97290950744599947, 14.00000000000000000 ) ) ;
#13157 = EDGE_LOOP ( 'NONE', ( #13748, #12772 ) ) ;
#13158 = AXIS2_PLACEMENT_3D ( 'NONE', #9128, #7928, #535 ) ;
#13159 = CIRCLE ( 'NONE', #4032, 3.000000000000000000 ) ;
#13160 = ORIENTED_EDGE ( 'NONE', *, *, #5121, .F. ) ;
#13161 = EDGE_LOOP ( 'NONE', ( #1430, #3280 ) ) ;
#13162 = ORIENTED_EDGE ( 'NONE', *, *, #562, .T. ) ;
#13163 = CARTESIAN_POINT ( 'NONE',  ( -25.22489219260310023, -4.443078545630350540, 62.14999999999999858 ) ) ;
#13164 = ORIENTED_EDGE ( 'NONE', *, *, #11225, .T. ) ;
#13165 = ORIENTED_EDGE ( 'NONE', *, *, #3592, .T. ) ;
#13166 = CARTESIAN_POINT ( 'NONE',  ( -18.05918829504999934, 10.97290950744599947, 116.8499999999999943 ) ) ;
#13167 = CARTESIAN_POINT ( 'NONE',  ( -21.30030954502889173, 30.13305483534595197, 59.66158781348052997 ) ) ;
#13168 = DIRECTION ( 'NONE',  ( -1.000000000000000000, -0.000000000000000000, -0.000000000000000000 ) ) ;
#13169 = CARTESIAN_POINT ( 'NONE',  ( -18.05918829504999934, 10.97290950744599947, 60.04999999999999716 ) ) ;
#13170 = LINE ( 'NONE', #11081, #6208 ) ;
#13171 = LINE ( 'NONE', #7782, #1127 ) ;
#13172 = CARTESIAN_POINT ( 'NONE',  ( 50.63563590245420443, 103.9054980190242361, 20.00000000000000000 ) ) ;
#13173 = VECTOR ( 'NONE', #3631, 1000.000000000000000 ) ;
#13174 = VECTOR ( 'NONE', #13751, 1000.000000000000000 ) ;
#13175 = AXIS2_PLACEMENT_3D ( 'NONE', #9181, #3877, #13433 ) ;
#13176 = CIRCLE ( 'NONE', #12287, 6.145833333000000565 ) ;
#13177 = EDGE_CURVE ( 'NONE', #12897, #7297, #12878, .T. ) ;
#13178 = ORIENTED_EDGE ( 'NONE', *, *, #12847, .T. ) ;
#13179 = CIRCLE ( 'NONE', #4272, 0.7500000000000006661 ) ;
#13180 = DIRECTION ( 'NONE',  ( 1.000000000000000000, 0.000000000000000000, 0.000000000000000000 ) ) ;
#13181 = PLANE ( 'NONE',  #8466 ) ;
#13182 = AXIS2_PLACEMENT_3D ( 'NONE', #1499, #5754, #12131 ) ;
#13183 = EDGE_LOOP ( 'NONE', ( #3522, #7184, #1030, #3555 ) ) ;
#13184 = LINE ( 'NONE', #8995, #13173 ) ;
#13185 = DIRECTION ( 'NONE',  ( -0.000000000000000000, 1.000000000000000000, -0.000000000000000000 ) ) ;
#13186 = CARTESIAN_POINT ( 'NONE',  ( 3.940811704950010430, -11.02709049255400053, 0.000000000000000000 ) ) ;
#13187 = DIRECTION ( 'NONE',  ( 1.000000000000000000, 0.000000000000000000, 0.000000000000000000 ) ) ;
#13188 = DIRECTION ( 'NONE',  ( 1.000000000000000000, 0.000000000000000000, 0.000000000000000000 ) ) ;
#13189 = DIRECTION ( 'NONE',  ( 0.000000000000000000, 0.000000000000000000, 1.000000000000000000 ) ) ;
#13190 = DIRECTION ( 'NONE',  ( -1.000000000000000000, 0.000000000000000000, 0.000000000000000000 ) ) ;
#13191 = DIRECTION ( 'NONE',  ( 0.000000000000000000, 0.000000000000000000, 1.000000000000000000 ) ) ;
#13192 = DIRECTION ( 'NONE',  ( 0.000000000000000000, 0.000000000000000000, -1.000000000000000000 ) ) ;
#13193 = LINE ( 'NONE', #8861, #10902 ) ;
#13194 = EDGE_CURVE ( 'NONE', #11014, #7637, #835, .T. ) ;
#13195 = SHAPE_REPRESENTATION ( 'compact pneumatic cylinder', ( #6434 ), #5097 ) ;
#13196 = CIRCLE ( 'NONE', #4283, 34.70000000000000284 ) ;
#13197 = ORIENTED_EDGE ( 'NONE', *, *, #7104, .F. ) ;
#13198 = ORIENTED_EDGE ( 'NONE', *, *, #12315, .F. ) ;
#13199 = DIRECTION ( 'NONE',  ( -0.000000000000000000, -0.000000000000000000, -1.000000000000000000 ) ) ;
#13200 = ORIENTED_EDGE ( 'NONE', *, *, #11241, .T. ) ;
#13201 = EDGE_LOOP ( 'NONE', ( #9442, #2993, #3218, #13597 ) ) ;
#13202 = ORIENTED_EDGE ( 'NONE', *, *, #3433, .T. ) ;
#13203 = CARTESIAN_POINT ( 'NONE',  ( 134.6356359024541973, 103.9054980190242361, 22.89644660940672694 ) ) ;
#13204 = PRESENTATION_LAYER_ASSIGNMENT (  '', '', ( #5833 ) ) ;
#13205 = CARTESIAN_POINT ( 'NONE',  ( 140.6356359024541689, 85.03908161011133870, 0.7500000000000006661 ) ) ;
#13206 = DIRECTION ( 'NONE',  ( 1.000000000000000000, 0.000000000000000000, 0.000000000000000000 ) ) ;
#13207 = DIRECTION ( 'NONE',  ( 0.000000000000000000, -1.000000000000000000, 0.000000000000000000 ) ) ;
#13208 = ADVANCED_FACE ( 'NONE', ( #5325 ), #8345, .F. ) ;
#13209 = DIRECTION ( 'NONE',  ( 1.577021341797097560E-16, -1.000000000000000000, 0.000000000000000000 ) ) ;
#13210 = EDGE_CURVE ( 'NONE', #6644, #8435, #9756, .T. ) ;
#13211 = CIRCLE ( 'NONE', #716, 1.999999999999989564 ) ;
#13212 = VERTEX_POINT ( 'NONE', #7340 ) ;
#13213 = ORIENTED_EDGE ( 'NONE', *, *, #6328, .T. ) ;
#13214 = EDGE_CURVE ( 'NONE', #1934, #2494, #2195, .T. ) ;
#13215 = EDGE_LOOP ( 'NONE', ( #10313, #1939, #12217, #13059 ) ) ;
#13216 = EDGE_CURVE ( 'NONE', #3609, #13362, #9538, .T. ) ;
#13217 = DIRECTION ( 'NONE',  ( 1.000000000000000000, 0.000000000000000000, 0.000000000000000000 ) ) ;
#13218 = VERTEX_POINT ( 'NONE', #5791 ) ;
#13219 = VERTEX_POINT ( 'NONE', #12373 ) ;
#13220 = ORIENTED_EDGE ( 'NONE', *, *, #7980, .F. ) ;
#13221 = ORIENTED_EDGE ( 'NONE', *, *, #12977, .F. ) ;
#13222 = ORIENTED_EDGE ( 'NONE', *, *, #4782, .T. ) ;
#13223 = FACE_OUTER_BOUND ( 'NONE', #3574, .T. ) ;
#13224 = LINE ( 'NONE', #3665, #3752 ) ;
#13225 = EDGE_LOOP ( 'NONE', ( #1699, #2782, #1379, #2593 ) ) ;
#13226 = DIRECTION ( 'NONE',  ( -0.000000000000000000, -0.000000000000000000, 1.000000000000000000 ) ) ;
#13227 = DIRECTION ( 'NONE',  ( 0.000000000000000000, 0.000000000000000000, -1.000000000000000000 ) ) ;
#13228 = CARTESIAN_POINT ( 'NONE',  ( -18.05918829504999934, 10.97290950744599947, 60.85000000000000142 ) ) ;
#13229 = EDGE_CURVE ( 'NONE', #1301, #4724, #7503, .T. ) ;
#13230 = DIRECTION ( 'NONE',  ( 0.000000000000000000, 0.000000000000000000, 1.000000000000000000 ) ) ;
#13231 = VERTEX_POINT ( 'NONE', #9074 ) ;
#13232 = EDGE_CURVE ( 'NONE', #11929, #719, #11905, .T. ) ;
#13233 = CIRCLE ( 'NONE', #1406, 16.00000000000000000 ) ;
#13234 = ORIENTED_EDGE ( 'NONE', *, *, #10084, .T. ) ;
#13235 = EDGE_LOOP ( 'NONE', ( #4121, #3932, #5743, #8602 ) ) ;
#13236 = CARTESIAN_POINT ( 'NONE',  ( -3.499999999999998224, 2.499999999999999556, -65.00000000000000000 ) ) ;
#13237 = VERTEX_POINT ( 'NONE', #501 ) ;
#13238 = DIRECTION ( 'NONE',  ( -0.000000000000000000, -0.000000000000000000, 1.000000000000000000 ) ) ;
#13239 = CARTESIAN_POINT ( 'NONE',  ( -21.89015644058605758, 30.04220389462367891, 56.84109027995026509 ) ) ;
#13240 = CARTESIAN_POINT ( 'NONE',  ( 50.63563590245420443, 103.9054980190242361, 22.75000000000000000 ) ) ;
#13241 = DIRECTION ( 'NONE',  ( -0.000000000000000000, 1.000000000000000000, -0.000000000000000000 ) ) ;
#13242 = LINE ( 'NONE', #3682, #3620 ) ;
#13243 = CONICAL_SURFACE ( 'NONE', #6000, 16.95000000000000284, 0.7853981633974447263 ) ;
#13244 = DIRECTION ( 'NONE',  ( 0.000000000000000000, 0.000000000000000000, 1.000000000000000000 ) ) ;
#13245 = EDGE_CURVE ( 'NONE', #898, #10213, #9996, .T. ) ;
#13246 = DIRECTION ( 'NONE',  ( -0.9496839325805410681, 0.3132098788326420080, 0.000000000000000000 ) ) ;
#13247 = DIRECTION ( 'NONE',  ( 1.000000000000000000, 0.000000000000000000, 0.000000000000000000 ) ) ;
#13248 = CARTESIAN_POINT ( 'NONE',  ( -18.05918829504999934, 10.97290950744599947, 61.86500000000000199 ) ) ;
#13249 = CYLINDRICAL_SURFACE ( 'NONE', #5069, 2.500000000000000000 ) ;
#13250 = CARTESIAN_POINT ( 'NONE',  ( -18.05918829504999934, 10.97290950744599947, 63.02000000000000313 ) ) ;
#13251 = CARTESIAN_POINT ( 'NONE',  ( 62.16596598834396303, 68.56941169600129626, 0.7500000000000000000 ) ) ;
#13252 = CARTESIAN_POINT ( 'NONE',  ( -7.640422211807256225, -16.89844320975769776, -3.000000000000000000 ) ) ;
#13253 = CARTESIAN_POINT ( 'NONE',  ( -35.05918829505000645, -6.027090492554000534, 64.85000000000000853 ) ) ;
#13254 = FACE_OUTER_BOUND ( 'NONE', #2100, .T. ) ;
#13255 = DIRECTION ( 'NONE',  ( 0.000000000000000000, 0.000000000000000000, -1.000000000000000000 ) ) ;
#13256 = CARTESIAN_POINT ( 'NONE',  ( -38.05918829505000645, 27.97290950744599769, 10.00000000000000000 ) ) ;
#13257 = CARTESIAN_POINT ( 'NONE',  ( -36.05918829505000645, 10.97290950744599947, 62.14999999999999858 ) ) ;
#13258 = ORIENTED_EDGE ( 'NONE', *, *, #7920, .T. ) ;
#13259 = CARTESIAN_POINT ( 'NONE',  ( 43.38563590245419732, 110.7284214383315089, 0.000000000000000000 ) ) ;
#13260 = EDGE_CURVE ( 'NONE', #10544, #11762, #3767, .T. ) ;
#13261 = EDGE_CURVE ( 'NONE', #3141, #1834, #3536, .T. ) ;
#13262 = VERTEX_POINT ( 'NONE', #7620 ) ;
#13263 = DIRECTION ( 'NONE',  ( 0.000000000000000000, 0.000000000000000000, -1.000000000000000000 ) ) ;
#13264 = FACE_OUTER_BOUND ( 'NONE', #5221, .T. ) ;
#13265 = DIRECTION ( 'NONE',  ( 0.000000000000000000, 0.000000000000000000, 1.000000000000000000 ) ) ;
#13266 = VERTEX_POINT ( 'NONE', #11970 ) ;
#13267 = ADVANCED_FACE ( 'NONE', ( #13335 ), #12750, .T. ) ;
#13268 = DIRECTION ( 'NONE',  ( 0.4528443260392608916, 0.8915896008669279560, 0.000000000000000000 ) ) ;
#13269 =( BOUNDED_SURFACE ( )  B_SPLINE_SURFACE ( 3, 3, ( 
 ( #8045, #640, #2561, #9941 ),
 ( #13426, #368, #575, #9174 ),
 ( #11128, #5806, #11202, #3599 ),
 ( #12325, #4776, #3870, #7968 ) ),
 .UNSPECIFIED., .F., .F., .T. ) 
 B_SPLINE_SURFACE_WITH_KNOTS ( ( 4, 4 ),
 ( 4, 4 ),
 ( 0.000000000000000000, 1.000000000000000000 ),
 ( 0.000000000000000000, 1.000000000000000000 ),
 .UNSPECIFIED. ) 
 GEOMETRIC_REPRESENTATION_ITEM ( )  RATIONAL_B_SPLINE_SURFACE ( (
 ( 1.000000000000000000, 0.3333333333333329818, 0.3333333333333329818, 1.000000000000000000),
 ( 0.4470472315060959878, 0.1490157438353659769, 0.1490157438353659769, 0.4470472315060959878),
 ( 0.4470472315060959878, 0.1490157438353659769, 0.1490157438353659769, 0.4470472315060959878),
 ( 1.000000000000000000, 0.3333333333333329818, 0.3333333333333329818, 1.000000000000000000) ) ) 
 REPRESENTATION_ITEM ( '' )  SURFACE ( )  );
#13270 = DIRECTION ( 'NONE',  ( 1.000000000000000000, 0.000000000000000000, 0.000000000000000000 ) ) ;
#13271 = DIRECTION ( 'NONE',  ( -1.000000000000000000, 0.000000000000000000, 0.000000000000000000 ) ) ;
#13272 = CARTESIAN_POINT ( 'NONE',  ( -1.396365658198039927, 10.97290950744599947, 6.250000000000000000 ) ) ;
#13273 = ORIENTED_EDGE ( 'NONE', *, *, #9951, .F. ) ;
#13274 = AXIS2_PLACEMENT_3D ( 'NONE', #10200, #7808, #617 ) ;
#13275 = EDGE_LOOP ( 'NONE', ( #13001, #8536 ) ) ;
#13276 = CARTESIAN_POINT ( 'NONE',  ( -16.30032143609284034, 30.29381900179400589, 61.21967481679787682 ) ) ;
#13277 = EDGE_CURVE ( 'NONE', #8708, #349, #153, .T. ) ;
#13278 = ORIENTED_EDGE ( 'NONE', *, *, #2343, .F. ) ;
#13279 = ORIENTED_EDGE ( 'NONE', *, *, #8938, .F. ) ;
#13280 = EDGE_LOOP ( 'NONE', ( #4811, #1956, #117, #4610 ) ) ;
#13281 = FACE_BOUND ( 'NONE', #3171, .T. ) ;
#13282 = ORIENTED_EDGE ( 'NONE', *, *, #8256, .T. ) ;
#13283 = ADVANCED_FACE ( 'NONE', ( #8107 ), #13413, .T. ) ;
#13284 = CYLINDRICAL_SURFACE ( 'NONE', #8226, 2.700000000000000178 ) ;
#13285 = DIRECTION ( 'NONE',  ( 0.000000000000000000, 0.000000000000000000, 1.000000000000000000 ) ) ;
#13286 = VERTEX_POINT ( 'NONE', #4760 ) ;
#13287 = EDGE_CURVE ( 'NONE', #4217, #6494, #1065, .T. ) ;
#13288 = CYLINDRICAL_SURFACE ( 'NONE', #11642, 2.000000000000001776 ) ;
#13289 = CARTESIAN_POINT ( 'NONE',  ( 0.4408117049500004381, 10.97290950744600124, 11.50000000000000000 ) ) ;
#13290 = CARTESIAN_POINT ( 'NONE',  ( -19.55918829504999934, 27.19822998463872565, 57.14449823292531505 ) ) ;
#13291 = ADVANCED_FACE ( 'NONE', ( #9815, #12229, #13015 ), #6653, .T. ) ;
#13292 = VECTOR ( 'NONE', #4999, 1000.000000000000000 ) ;
#13293 = DIRECTION ( 'NONE',  ( 0.000000000000000000, 0.000000000000000000, -1.000000000000000000 ) ) ;
#13294 = EDGE_LOOP ( 'NONE', ( #11461, #11662, #3886, #7693 ) ) ;
#13295 = EDGE_LOOP ( 'NONE', ( #7405, #7457, #12478, #13737, #6174 ) ) ;
#13296 = EDGE_CURVE ( 'NONE', #6971, #719, #10341, .T. ) ;
#13297 = CIRCLE ( 'NONE', #1032, 16.75000000000000355 ) ;
#13298 = CARTESIAN_POINT ( 'NONE',  ( 68.49370948373500312, 85.03908161011133870, 20.00000000000000000 ) ) ;
#13299 = FILL_AREA_STYLE ('',( #3540 ) ) ;
#13300 = EDGE_CURVE ( 'NONE', #10154, #6107, #12454, .T. ) ;
#13301 = CARTESIAN_POINT ( 'NONE',  ( -20.84843554743573435, 30.19221003206969201, 54.37310230029029157 ) ) ;
#13302 = CARTESIAN_POINT ( 'NONE',  ( -20.04397650943645459, 13.22249074492834175, 24.10000000000000142 ) ) ;
#13303 = LINE ( 'NONE', #5623, #10655 ) ;
#13304 = CARTESIAN_POINT ( 'NONE',  ( 68.49370948373500312, 112.2890816101113387, 19.25000000000000000 ) ) ;
#13305 = DIRECTION ( 'NONE',  ( -1.000000000000000000, -0.000000000000000000, -0.000000000000000000 ) ) ;
#13306 = EDGE_CURVE ( 'NONE', #2826, #8318, #7986, .T. ) ;
#13307 = CARTESIAN_POINT ( 'NONE',  ( -30.80918829504999934, 27.97290950744599769, 58.85000000000000142 ) ) ;
#13308 = EDGE_CURVE ( 'NONE', #9491, #3613, #5672, .T. ) ;
#13309 = CARTESIAN_POINT ( 'NONE',  ( -18.05918829504999934, 10.97290950744599947, 68.84999999999999432 ) ) ;
#13310 = LINE ( 'NONE', #12276, #5122 ) ;
#13311 = CARTESIAN_POINT ( 'NONE',  ( -23.57208814848684852, -7.366404416634599883, 62.14999999999999858 ) ) ;
#13312 = FILL_AREA_STYLE ('',( #3632 ) ) ;
#13313 = AXIS2_PLACEMENT_3D ( 'NONE', #9418, #8082, #3834 ) ;
#13314 = CYLINDRICAL_SURFACE ( 'NONE', #10966, 5.000000000000000888 ) ;
#13315 = CARTESIAN_POINT ( 'NONE',  ( -22.67016924028392921, 13.57258417831237729, 68.55666012861996705 ) ) ;
#13316 = CARTESIAN_POINT ( 'NONE',  ( -4.599650328638321461, 0.000000000000000000, -7.878124499050794149 ) ) ;
#13317 = DIRECTION ( 'NONE',  ( 0.000000000000000000, 0.000000000000000000, 1.000000000000000000 ) ) ;
#13318 = DIRECTION ( 'NONE',  ( -1.000000000000000000, -1.239088197126292296E-16, 0.000000000000000000 ) ) ;
#13319 = EDGE_CURVE ( 'NONE', #9911, #2900, #8312, .T. ) ;
#13320 = DIRECTION ( 'NONE',  ( -1.000000000000000000, 0.000000000000000000, 0.000000000000000000 ) ) ;
#13321 = FACE_OUTER_BOUND ( 'NONE', #1649, .T. ) ;
#13322 = ADVANCED_FACE ( 'NONE', ( #1827 ), #5023, .T. ) ;
#13323 = AXIS2_PLACEMENT_3D ( 'NONE', #11281, #7005, #13572 ) ;
#13324 = EDGE_LOOP ( 'NONE', ( #10528, #5109, #3491, #3024 ) ) ;
#13325 = EDGE_LOOP ( 'NONE', ( #2810, #7011, #6533 ) ) ;
#13326 = CARTESIAN_POINT ( 'NONE',  ( 92.63563590245421153, 99.03908161011133870, 20.00000000000000000 ) ) ;
#13327 = ORIENTED_EDGE ( 'NONE', *, *, #3990, .F. ) ;
#13328 = ORIENTED_EDGE ( 'NONE', *, *, #9899, .F. ) ;
#13329 = CARTESIAN_POINT ( 'NONE',  ( 142.1053058165643108, 110.5087515242214096, 0.000000000000000000 ) ) ;
#13330 = CARTESIAN_POINT ( 'NONE',  ( 50.63563590245420443, 94.90549801902425031, 22.75000000000000000 ) ) ;
#13331 = CIRCLE ( 'NONE', #10445, 2.000000000000001776 ) ;
#13332 = DIRECTION ( 'NONE',  ( -0.000000000000000000, -0.000000000000000000, -1.000000000000000000 ) ) ;
#13333 = AXIS2_PLACEMENT_3D ( 'NONE', #479, #1384, #7720 ) ;
#13334 = CARTESIAN_POINT ( 'NONE',  ( 18.45469220996244886, 1.832421873814834123, 0.000000000000000000 ) ) ;
#13335 = FACE_OUTER_BOUND ( 'NONE', #233, .T. ) ;
#13336 = DIRECTION ( 'NONE',  ( -1.000000000000000000, 0.000000000000000000, 0.000000000000000000 ) ) ;
#13337 = DIRECTION ( 'NONE',  ( 0.000000000000000000, 0.000000000000000000, 1.000000000000000000 ) ) ;
#13338 = EDGE_CURVE ( 'NONE', #11332, #6506, #2668, .T. ) ;
#13339 = AXIS2_PLACEMENT_3D ( 'NONE', #7095, #5976, #6117 ) ;
#13340 = CIRCLE ( 'NONE', #10462, 16.00000000000000000 ) ;
#13341 = VECTOR ( 'NONE', #3694, 1000.000000000000114 ) ;
#13342 = CIRCLE ( 'NONE', #1758, 4.749999999999997335 ) ;
#13343 = VERTEX_POINT ( 'NONE', #768 ) ;
#13344 = LINE ( 'NONE', #2554, #4579 ) ;
#13345 = EDGE_LOOP ( 'NONE', ( #9592, #11691 ) ) ;
#13346 = ORIENTED_EDGE ( 'NONE', *, *, #9760, .T. ) ;
#13347 = ORIENTED_EDGE ( 'NONE', *, *, #2914, .T. ) ;
#13348 = DIRECTION ( 'NONE',  ( 1.000000000000000000, 3.574581708073420512E-15, 0.000000000000000000 ) ) ;
#13349 = DIRECTION ( 'NONE',  ( 0.000000000000000000, 0.000000000000000000, -1.000000000000000000 ) ) ;
#13350 = CARTESIAN_POINT ( 'NONE',  ( 12.00000000000000000, -2.499999999999999556, 0.000000000000000000 ) ) ;
#13351 = ORIENTED_EDGE ( 'NONE', *, *, #12167, .T. ) ;
#13352 = CARTESIAN_POINT ( 'NONE',  ( -25.73489962141544751, -4.139534227248430120, 58.35000000000000142 ) ) ;
#13353 = AXIS2_PLACEMENT_3D ( 'NONE', #12152, #12565, #13595 ) ;
#13354 = CARTESIAN_POINT ( 'NONE',  ( -8.964285665223000521, 0.3335619008453594714, 63.45000000000000284 ) ) ;
#13355 = AXIS2_PLACEMENT_3D ( 'NONE', #5092, #1964, #979 ) ;
#13356 = LINE ( 'NONE', #12115, #9581 ) ;
#13357 = AXIS2_PLACEMENT_3D ( 'NONE', #9340, #809, #12623 ) ;
#13358 = CARTESIAN_POINT ( 'NONE',  ( 134.8856359024541973, 89.90549801902423610, 23.00000000000000000 ) ) ;
#13359 = ADVANCED_FACE ( 'NONE', ( #13744 ), #5094, .T. ) ;
#13360 = PRODUCT_DEFINITION_FORMATION_WITH_SPECIFIED_SOURCE ( 'ANY', '', #3300, .NOT_KNOWN. ) ;
#13361 = ORIENTED_EDGE ( 'NONE', *, *, #820, .F. ) ;
#13362 = VERTEX_POINT ( 'NONE', #9294 ) ;
#13363 = CARTESIAN_POINT ( 'NONE',  ( 50.63563590245420443, 94.65549801902425031, 22.75000000000000000 ) ) ;
#13364 = VECTOR ( 'NONE', #7197, 1000.000000000000000 ) ;
#13365 = AXIS2_PLACEMENT_3D ( 'NONE', #11025, #7643, #7854 ) ;
#13366 = EDGE_CURVE ( 'NONE', #8674, #5058, #4069, .T. ) ;
#13367 = TOROIDAL_SURFACE ( 'NONE', #3132, 16.66282263685194920, 1.000000000000000000 ) ;
#13368 = DIRECTION ( 'NONE',  ( 0.000000000000000000, -1.000000000000000000, 1.672022627447524796E-15 ) ) ;
#13369 = CARTESIAN_POINT ( 'NONE',  ( -21.88875334366193570, 30.04243591130237689, 57.61769108546867102 ) ) ;
#13370 = LINE ( 'NONE', #7072, #2989 ) ;
#13371 = PLANE ( 'NONE',  #7977 ) ;
#13372 = CARTESIAN_POINT ( 'NONE',  ( 2.262399129208275017, -0.4981161769137599782, 17.25000000000000000 ) ) ;
#13373 = DIRECTION ( 'NONE',  ( 0.000000000000000000, 0.000000000000000000, -1.000000000000000000 ) ) ;
#13374 = CARTESIAN_POINT ( 'NONE',  ( -56.55918829505007750, 8.972909507445617550, 163.8499999999999943 ) ) ;
#13375 = VERTEX_POINT ( 'NONE', #9498 ) ;
#13376 = ADVANCED_FACE ( 'NONE', ( #694 ), #3031, .T. ) ;
#13377 = AXIS2_PLACEMENT_3D ( 'NONE', #7112, #1678, #7043 ) ;
#13378 = CIRCLE ( 'NONE', #4915, 18.00000000000000000 ) ;
#13379 = EDGE_CURVE ( 'NONE', #10213, #7294, #8207, .T. ) ;
#13380 = CARTESIAN_POINT ( 'NONE',  ( -18.05918829504999934, 10.97290950744599947, 64.85000000000000853 ) ) ;
#13381 = DIRECTION ( 'NONE',  ( -1.000000000000000000, 0.000000000000000000, 0.000000000000000000 ) ) ;
#13382 = ORIENTED_EDGE ( 'NONE', *, *, #2498, .F. ) ;
#13383 = DIRECTION ( 'NONE',  ( 0.000000000000000000, 0.000000000000000000, -1.000000000000000000 ) ) ;
#13384 = CARTESIAN_POINT ( 'NONE',  ( -12.00918829505000041, 10.97290950744599947, 64.85000000000000853 ) ) ;
#13385 = DIRECTION ( 'NONE',  ( 0.000000000000000000, 0.000000000000000000, -1.000000000000000000 ) ) ;
#13386 = CARTESIAN_POINT ( 'NONE',  ( -18.05918829504999934, 10.97290950744599947, 7.250000000000000000 ) ) ;
#13387 = AXIS2_PLACEMENT_3D ( 'NONE', #2387, #8718, #4740 ) ;
#13388 = LINE ( 'NONE', #3837, #8518 ) ;
#13389 = DIRECTION ( 'NONE',  ( 1.000000000000000000, 0.000000000000000000, 0.000000000000000000 ) ) ;
#13390 = CONICAL_SURFACE ( 'NONE', #7347, 16.00000000000000000, 0.7853981633974476129 ) ;
#13391 = FACE_OUTER_BOUND ( 'NONE', #251, .T. ) ;
#13392 = FACE_OUTER_BOUND ( 'NONE', #9895, .T. ) ;
#13393 = CARTESIAN_POINT ( 'NONE',  ( 50.38563590245420443, 94.65549801902425031, 23.00000000000000000 ) ) ;
#13394 = PLANE ( 'NONE',  #4882 ) ;
#13395 = EDGE_CURVE ( 'NONE', #11676, #3610, #4963, .T. ) ;
#13396 = UNCERTAINTY_MEASURE_WITH_UNIT (LENGTH_MEASURE( 1.000000000000000082E-05 ), #4550, 'distance_accuracy_value', 'NONE');
#13397 = AXIS2_PLACEMENT_3D ( 'NONE', #10804, #9089, #3792 ) ;
#13398 = AXIS2_PLACEMENT_3D ( 'NONE', #12071, #9055, #2592 ) ;
#13399 = AXIS2_PLACEMENT_3D ( 'NONE', #5214, #9548, #13523 ) ;
#13400 = ORIENTED_EDGE ( 'NONE', *, *, #2910, .F. ) ;
#13401 = EDGE_CURVE ( 'NONE', #8804, #2573, #12007, .T. ) ;
#13402 = EDGE_LOOP ( 'NONE', ( #10223, #10047 ) ) ;
#13403 = CARTESIAN_POINT ( 'NONE',  ( 10.81426999815522549, -15.06602133594279991, 7.000000000000000000 ) ) ;
#13404 = ORIENTED_EDGE ( 'NONE', *, *, #9449, .F. ) ;
#13405 = ORIENTED_EDGE ( 'NONE', *, *, #12125, .T. ) ;
#13406 = EDGE_LOOP ( 'NONE', ( #13143, #6902 ) ) ;
#13407 = FACE_OUTER_BOUND ( 'NONE', #11687, .T. ) ;
#13408 = LINE ( 'NONE', #3854, #10495 ) ;
#13409 = FILL_AREA_STYLE ('',( #6199 ) ) ;
#13410 = DIRECTION ( 'NONE',  ( 0.000000000000000000, 0.000000000000000000, 1.000000000000000000 ) ) ;
#13411 = VECTOR ( 'NONE', #9155, 1000.000000000000000 ) ;
#13412 = VECTOR ( 'NONE', #6319, 1000.000000000000000 ) ;
#13413 = CYLINDRICAL_SURFACE ( 'NONE', #411, 34.69999999999999574 ) ;
#13414 = AXIS2_PLACEMENT_3D ( 'NONE', #3058, #7273, #11485 ) ;
#13415 = DIRECTION ( 'NONE',  ( -0.000000000000000000, 0.000000000000000000, -1.000000000000000000 ) ) ;
#13416 = CARTESIAN_POINT ( 'NONE',  ( -18.05918829504999934, 10.97290950744599947, 57.35000000000000142 ) ) ;
#13417 = ORIENTED_EDGE ( 'NONE', *, *, #13454, .T. ) ;
#13418 = ORIENTED_EDGE ( 'NONE', *, *, #6998, .T. ) ;
#13419 = CARTESIAN_POINT ( 'NONE',  ( -15.94002774258076016, 30.26343021274545109, 60.97416097055285178 ) ) ;
#13420 = AXIS2_PLACEMENT_3D ( 'NONE', #8970, #3668, #5666 ) ;
#13421 = ORIENTED_EDGE ( 'NONE', *, *, #1485, .T. ) ;
#13422 = VERTEX_POINT ( 'NONE', #5996 ) ;
#13423 = SURFACE_SIDE_STYLE ('',( #1763 ) ) ;
#13424 = DIRECTION ( 'NONE',  ( 1.239088197126291063E-16, 1.000000000000000000, -0.000000000000000000 ) ) ;
#13425 = EDGE_LOOP ( 'NONE', ( #13790, #4166, #5488, #3220 ) ) ;
#13426 = CARTESIAN_POINT ( 'NONE',  ( -18.05918829505001355, 18.23680593644599668, 62.03182374100007479 ) ) ;
#13427 = EDGE_CURVE ( 'NONE', #8398, #1604, #1284, .T. ) ;
#13428 = DIRECTION ( 'NONE',  ( -1.000000000000000000, 0.000000000000000000, -0.000000000000000000 ) ) ;
#13429 = VERTEX_POINT ( 'NONE', #5168 ) ;
#13430 = CARTESIAN_POINT ( 'NONE',  ( -1.059188295049996231, 27.97290950744599769, 7.250000000000000000 ) ) ;
#13431 = CARTESIAN_POINT ( 'NONE',  ( -18.05918829504999934, 10.97290950744599947, 14.00000000000000000 ) ) ;
#13432 = DIRECTION ( 'NONE',  ( 0.000000000000000000, 0.000000000000000000, 1.000000000000000000 ) ) ;
#13433 = DIRECTION ( 'NONE',  ( -1.000000000000000000, 0.000000000000000000, 0.000000000000000000 ) ) ;
#13434 = AXIS2_PLACEMENT_3D ( 'NONE', #2156, #5471, #7778 ) ;
#13435 =( BOUNDED_CURVE ( )  B_SPLINE_CURVE ( 3, ( #10590, #102, #8556, #3332 ),
 .UNSPECIFIED., .F., .F. ) 
 B_SPLINE_CURVE_WITH_KNOTS ( ( 4, 4 ),
 ( 1.570796326794896558, 3.141592653589793560 ),
 .UNSPECIFIED. ) 
 CURVE ( )  GEOMETRIC_REPRESENTATION_ITEM ( )  RATIONAL_B_SPLINE_CURVE ( ( 1.000000000000000000, 0.8047378541243649375, 0.8047378541243649375, 1.000000000000000000 ) ) 
 REPRESENTATION_ITEM ( '' )  );
#13436 = CIRCLE ( 'NONE', #3861, 12.00000000000000355 ) ;
#13437 = VERTEX_POINT ( 'NONE', #9229 ) ;
#13438 = ADVANCED_FACE ( 'NONE', ( #12503 ), #9439, .T. ) ;
#13439 = EDGE_LOOP ( 'NONE', ( #13087, #2456 ) ) ;
#13440 = ADVANCED_FACE ( 'NONE', ( #2963 ), #7180, .T. ) ;
#13441 = CARTESIAN_POINT ( 'NONE',  ( -16.45469220996245596, -1.832421873814834123, 7.000000000000000000 ) ) ;
#13442 = DIRECTION ( 'NONE',  ( 0.000000000000000000, 0.000000000000000000, -1.000000000000000000 ) ) ;
#13443 = DIRECTION ( 'NONE',  ( 0.000000000000000000, 0.000000000000000000, 1.000000000000000000 ) ) ;
#13444 = EDGE_CURVE ( 'NONE', #13530, #11751, #13331, .T. ) ;
#13445 = CARTESIAN_POINT ( 'NONE',  ( -15.34212233881444831, 16.32244711264754855, 57.35000000000000142 ) ) ;
#13446 = LINE ( 'NONE', #11555, #11861 ) ;
#13447 = CARTESIAN_POINT ( 'NONE',  ( -16.55918829504999579, 27.40458623260099813, 57.35000000000000142 ) ) ;
#13448 = AXIS2_PLACEMENT_3D ( 'NONE', #579, #711, #1630 ) ;
#13449 = EDGE_CURVE ( 'NONE', #11622, #9491, #13052, .T. ) ;
#13450 = CARTESIAN_POINT ( 'NONE',  ( -18.05918829504999934, 10.97290950744599947, 64.54999999999999716 ) ) ;
#13451 = PLANE ( 'NONE',  #1951 ) ;
#13452 = EDGE_LOOP ( 'NONE', ( #5031, #7982, #2824, #1457 ) ) ;
#13453 = DIRECTION ( 'NONE',  ( 0.000000000000000000, 0.000000000000000000, -1.000000000000000000 ) ) ;
#13454 = EDGE_CURVE ( 'NONE', #1735, #11332, #4470, .T. ) ;
#13455 = CARTESIAN_POINT ( 'NONE',  ( -18.05918829504999934, 10.97290950744599947, 68.84999999999999432 ) ) ;
#13456 = CARTESIAN_POINT ( 'NONE',  ( -18.05918829504999934, 10.97290950744599947, 61.65000000000000568 ) ) ;
#13457 = CIRCLE ( 'NONE', #10344, 16.72262947720610171 ) ;
#13458 = DIRECTION ( 'NONE',  ( 0.000000000000000000, 0.000000000000000000, -1.000000000000000000 ) ) ;
#13459 = LINE ( 'NONE', #3903, #3853 ) ;
#13460 = CARTESIAN_POINT ( 'NONE',  ( 134.7391892930474739, 90.00905140961751272, 23.00000000000000000 ) ) ;
#13461 = EDGE_CURVE ( 'NONE', #5721, #11514, #6489, .T. ) ;
#13462 = CARTESIAN_POINT ( 'NONE',  ( -0.3963656581980404825, 10.97290950744599947, 5.250000000000000000 ) ) ;
#13463 = DIRECTION ( 'NONE',  ( 0.000000000000000000, 0.000000000000000000, -1.000000000000000000 ) ) ;
#13464 = ADVANCED_FACE ( 'NONE', ( #12907 ), #8726, .F. ) ;
#13465 = CARTESIAN_POINT ( 'NONE',  ( 50.63563590245420443, 94.90549801902423610, 22.89644660940672694 ) ) ;
#13466 = CARTESIAN_POINT ( 'NONE',  ( 81.82136590429890077, 114.1051029460540605, 10.00000000000000000 ) ) ;
#13467 = ADVANCED_FACE ( 'NONE', ( #10759 ), #12672, .F. ) ;
#13468 = EDGE_LOOP ( 'NONE', ( #7205, #10942, #9081, #12854 ) ) ;
#13469 = ORIENTED_EDGE ( 'NONE', *, *, #3063, .F. ) ;
#13470 = ORIENTED_EDGE ( 'NONE', *, *, #4163, .F. ) ;
#13471 = ORIENTED_EDGE ( 'NONE', *, *, #13565, .F. ) ;
#13472 = CYLINDRICAL_SURFACE ( 'NONE', #13499, 1.500000000000001332 ) ;
#13473 = ORIENTED_EDGE ( 'NONE', *, *, #5404, .T. ) ;
#13475 = EDGE_CURVE ( 'NONE', #51, #1551, #12232, .T. ) ;
#13474 = EDGE_LOOP ( 'NONE', ( #10410, #12084, #8892, #13704, #7842, #7371, #11961, #3170 ) ) ;
#13476 = DIRECTION ( 'NONE',  ( -1.000000000000000000, 0.000000000000000000, 0.000000000000000000 ) ) ;
#13477 = DIRECTION ( 'NONE',  ( -0.000000000000000000, -0.000000000000000000, 1.000000000000000000 ) ) ;
#13478 = CARTESIAN_POINT ( 'NONE',  ( -22.71804201037815218, -4.525318844826149878, 62.14999999999999858 ) ) ;
#13479 = CARTESIAN_POINT ( 'NONE',  ( -11.46335496205000126, 10.97290950744599947, 60.40999999999999659 ) ) ;
#13480 = CARTESIAN_POINT ( 'NONE',  ( -35.05918829505000645, -6.027090492554000534, 17.25000000000000000 ) ) ;
#13481 = DIRECTION ( 'NONE',  ( 0.000000000000000000, 0.000000000000000000, 1.000000000000000000 ) ) ;
#13482 = EDGE_CURVE ( 'NONE', #380, #2919, #11942, .T. ) ;
#13483 = DIRECTION ( 'NONE',  ( 0.000000000000000000, 0.000000000000000000, -1.000000000000000000 ) ) ;
#13484 = ORIENTED_EDGE ( 'NONE', *, *, #5793, .F. ) ;
#13485 = ORIENTED_EDGE ( 'NONE', *, *, #2571, .T. ) ;
#13486 = CARTESIAN_POINT ( 'NONE',  ( -15.35487948403739544, 30.20233709177388803, 60.42691889655178272 ) ) ;
#13487 = ORIENTED_EDGE ( 'NONE', *, *, #11392, .T. ) ;
#13488 = CONICAL_SURFACE ( 'NONE', #3919, 3.800000000000001155, 0.7853981633974476129 ) ;
#13489 = CARTESIAN_POINT ( 'NONE',  ( 16.04064420431708982, 4.500000000000000000, 9.307586582922137808 ) ) ;
#13490 = DIRECTION ( 'NONE',  ( -1.000000000000000000, 0.000000000000000000, 0.000000000000000000 ) ) ;
#13491 = EDGE_LOOP ( 'NONE', ( #12038, #9732 ) ) ;
#13492 = FACE_OUTER_BOUND ( 'NONE', #3051, .T. ) ;
#13493 = CARTESIAN_POINT ( 'NONE',  ( 0.04028432657539327000, 4.500000000000000000, -18.54539866546729243 ) ) ;
#13494 = ORIENTED_EDGE ( 'NONE', *, *, #5834, .F. ) ;
#13495 = CARTESIAN_POINT ( 'NONE',  ( -24.37001676333060018, -4.028726038184999858, 63.45000000000000284 ) ) ;
#13496 = DIRECTION ( 'NONE',  ( 0.000000000000000000, 0.000000000000000000, -1.000000000000000000 ) ) ;
#13497 = EDGE_CURVE ( 'NONE', #1261, #1264, #11877, .T. ) ;
#13498 = CARTESIAN_POINT ( 'NONE',  ( -1.059188295049996231, -6.027090492554000534, 64.35000000000000853 ) ) ;
#13499 = AXIS2_PLACEMENT_3D ( 'NONE', #1887, #686, #11311 ) ;
#13500 = ORIENTED_EDGE ( 'NONE', *, *, #7629, .F. ) ;
#13501 = DIRECTION ( 'NONE',  ( 0.7071067811865474617, 0.000000000000000000, 0.7071067811865474617 ) ) ;
#13502 = AXIS2_PLACEMENT_3D ( 'NONE', #1148, #2222, #6388 ) ;
#13503 = LINE ( 'NONE', #9190, #11411 ) ;
#13504 = DIRECTION ( 'NONE',  ( 1.000000000000000000, 0.000000000000000000, 0.000000000000000000 ) ) ;
#13505 = DIRECTION ( 'NONE',  ( 1.000000000000000000, 0.000000000000000000, 0.000000000000000000 ) ) ;
#13506 = DIRECTION ( 'NONE',  ( 0.000000000000000000, 0.000000000000000000, -1.000000000000000000 ) ) ;
#13507 = CARTESIAN_POINT ( 'NONE',  ( -18.05918829504999934, 10.97290950744599947, 61.86500000000000199 ) ) ;
#13508 = DIRECTION ( 'NONE',  ( 0.000000000000000000, 0.000000000000000000, 1.000000000000000000 ) ) ;
#13509 = ORIENTED_EDGE ( 'NONE', *, *, #12853, .T. ) ;
#13510 = ORIENTED_EDGE ( 'NONE', *, *, #12862, .T. ) ;
#13511 = ADVANCED_FACE ( 'NONE', ( #4270 ), #11117, .T. ) ;
#13512 = EDGE_CURVE ( 'NONE', #1130, #9971, #5744, .T. ) ;
#13513 = AXIS2_PLACEMENT_3D ( 'NONE', #11995, #396, #3686 ) ;
#13514 = DIRECTION ( 'NONE',  ( -0.000000000000000000, -0.000000000000000000, -1.000000000000000000 ) ) ;
#13515 = ORIENTED_EDGE ( 'NONE', *, *, #2424, .T. ) ;
#13516 = ORIENTED_EDGE ( 'NONE', *, *, #9250, .T. ) ;
#13517 = CARTESIAN_POINT ( 'NONE',  ( -18.05918829504999934, 10.97290950744599947, 64.54999999999999716 ) ) ;
#13518 = CARTESIAN_POINT ( 'NONE',  ( -1.059188295049996231, 27.97290950744599769, 64.85000000000000853 ) ) ;
#13519 = DIRECTION ( 'NONE',  ( 0.000000000000000000, 0.000000000000000000, -1.000000000000000000 ) ) ;
#13520 = CARTESIAN_POINT ( 'NONE',  ( 102.2760581142613603, 115.9375248198690826, 10.00000000000000000 ) ) ;
#13521 = CARTESIAN_POINT ( 'NONE',  ( -18.05918829504999934, 10.97290950744599947, 57.35000000000000142 ) ) ;
#13522 = LINE ( 'NONE', #8559, #3774 ) ;
#13523 = DIRECTION ( 'NONE',  ( -0.6615960714621568206, 0.7498604124941127269, 0.000000000000000000 ) ) ;
#13524 = VECTOR ( 'NONE', #4785, 1000.000000000000000 ) ;
#13525 = DIRECTION ( 'NONE',  ( -0.3202092937642119774, -0.6304490528084099044, -0.7071067811865499042 ) ) ;
#13526 = DIRECTION ( 'NONE',  ( 1.000000000000000000, 0.000000000000000000, 0.000000000000000000 ) ) ;
#13528 = EDGE_CURVE ( 'NONE', #8989, #13262, #12891, .T. ) ;
#13527 = PRODUCT_DEFINITION_CONTEXT ( 'detailed design', #3782, 'design' ) ;
#13529 = ADVANCED_FACE ( 'NONE', ( #11795 ), #1318, .T. ) ;
#13530 = VERTEX_POINT ( 'NONE', #283 ) ;
#13531 = AXIS2_PLACEMENT_3D ( 'NONE', #5161, #8437, #2958 ) ;
#13532 = EDGE_CURVE ( 'NONE', #7236, #9493, #4426, .T. ) ;
#13533 = CARTESIAN_POINT ( 'NONE',  ( 44.63563590245419732, 89.90549801902423610, 22.89644660940672694 ) ) ;
#13534 = EDGE_LOOP ( 'NONE', ( #5940, #12572, #10543, #6009 ) ) ;
#13535 = ORIENTED_EDGE ( 'NONE', *, *, #8545, .F. ) ;
#13536 = CARTESIAN_POINT ( 'NONE',  ( 8.000000000000001776, 2.000000000000000000, -65.00000000000000000 ) ) ;
#13537 = PRODUCT_RELATED_PRODUCT_CATEGORY ( 'part', '', ( #2255 ) ) ;
#13538 = CARTESIAN_POINT ( 'NONE',  ( -3.999999999999997335, 2.000000000000000000, -65.00000000000000000 ) ) ;
#13539 = DIRECTION ( 'NONE',  ( 0.000000000000000000, 0.000000000000000000, 1.000000000000000000 ) ) ;
#13540 = CARTESIAN_POINT ( 'NONE',  ( 50.63563590245420443, 108.9054980190242503, 20.00000000000000000 ) ) ;
#13541 = CARTESIAN_POINT ( 'NONE',  ( -18.05918829504999934, 10.97290950744599947, 63.64999999999999858 ) ) ;
#13542 = DIRECTION ( 'NONE',  ( 0.000000000000000000, 0.000000000000000000, -1.000000000000000000 ) ) ;
#13543 = VECTOR ( 'NONE', #4672, 1000.000000000000000 ) ;
#13544 = EDGE_CURVE ( 'NONE', #4291, #10303, #7439, .T. ) ;
#13545 = VERTEX_POINT ( 'NONE', #12779 ) ;
#13546 = VERTEX_POINT ( 'NONE', #3228 ) ;
#13547 = CARTESIAN_POINT ( 'NONE',  ( -14.80437462465609144, 30.13112197626990607, 55.06331687826421017 ) ) ;
#13548 = AXIS2_PLACEMENT_3D ( 'NONE', #1707, #11355, #8276 ) ;
#13549 = AXIS2_PLACEMENT_3D ( 'NONE', #10260, #670, #4942 ) ;
#13550 = VERTEX_POINT ( 'NONE', #6413 ) ;
#13551 = EDGE_LOOP ( 'NONE', ( #6982, #10945, #5016, #245 ) ) ;
#13552 = EDGE_CURVE ( 'NONE', #1905, #7929, #9707, .T. ) ;
#13553 = CARTESIAN_POINT ( 'NONE',  ( 12.00000000000000000, 2.500000000000000000, -65.00000000000000000 ) ) ;
#13554 = DIRECTION ( 'NONE',  ( -1.000000000000000000, 0.000000000000000000, 0.000000000000000000 ) ) ;
#13555 = ORIENTED_EDGE ( 'NONE', *, *, #1310, .T. ) ;
#13556 = CARTESIAN_POINT ( 'NONE',  ( -27.49999999999998934, 0.000000000000000000, 29.99999999999999645 ) ) ;
#13557 = LINE ( 'NONE', #2771, #5101 ) ;
#13558 = ORIENTED_EDGE ( 'NONE', *, *, #9153, .F. ) ;
#13559 = CARTESIAN_POINT ( 'NONE',  ( 123.1053058165639555, 68.56941169600116837, 19.25000000000000000 ) ) ;
#13560 = LINE ( 'NONE', #7659, #10565 ) ;
#13561 = CARTESIAN_POINT ( 'NONE',  ( -19.36881307809606056, 27.92256143814164560, 58.10788369877568016 ) ) ;
#13562 = DIRECTION ( 'NONE',  ( -0.000000000000000000, -0.000000000000000000, 1.000000000000000000 ) ) ;
#13563 = AXIS2_PLACEMENT_3D ( 'NONE', #8121, #6928, #1625 ) ;
#13564 = AXIS2_PLACEMENT_3D ( 'NONE', #13591, #810, #5008 ) ;
#13565 = EDGE_CURVE ( 'NONE', #1636, #10781, #6635, .T. ) ;
#13566 = AXIS2_PLACEMENT_3D ( 'NONE', #11063, #10927, #12109 ) ;
#13567 = ORIENTED_EDGE ( 'NONE', *, *, #13552, .F. ) ;
#13568 = VERTEX_POINT ( 'NONE', #2252 ) ;
#13569 = EDGE_CURVE ( 'NONE', #525, #8048, #11040, .T. ) ;
#13570 = CIRCLE ( 'NONE', #7304, 1.999999999999989564 ) ;
#13571 = AXIS2_PLACEMENT_3D ( 'NONE', #5342, #4319, #7483 ) ;
#13572 = DIRECTION ( 'NONE',  ( 1.000000000000000000, 0.000000000000000000, 0.000000000000000000 ) ) ;
#13573 = AXIS2_PLACEMENT_3D ( 'NONE', #11809, #74, #10770 ) ;
#13574 = ORIENTED_EDGE ( 'NONE', *, *, #11186, .T. ) ;
#13575 = PLANE ( 'NONE',  #7598 ) ;
#13576 = DIRECTION ( 'NONE',  ( 0.000000000000000000, 0.000000000000000000, 1.000000000000000000 ) ) ;
#13577 = FACE_BOUND ( 'NONE', #7677, .T. ) ;
#13578 = DIRECTION ( 'NONE',  ( 1.000000000000000000, 0.000000000000000000, 0.000000000000000000 ) ) ;
#13579 = DIRECTION ( 'NONE',  ( 0.000000000000000000, 0.000000000000000000, -1.000000000000000000 ) ) ;
#13580 =( NAMED_UNIT ( * ) PLANE_ANGLE_UNIT ( ) SI_UNIT ( $, .RADIAN. ) );
#13581 = VERTEX_POINT ( 'NONE', #9923 ) ;
#13582 = VECTOR ( 'NONE', #13698, 1000.000000000000000 ) ;
#13583 = CARTESIAN_POINT ( 'NONE',  ( 1.640811704950000172, 27.97290950744599769, 64.85000000000000853 ) ) ;
#13584 = VERTEX_POINT ( 'NONE', #5848 ) ;
#13585 = ORIENTED_EDGE ( 'NONE', *, *, #4099, .F. ) ;
#13586 = CARTESIAN_POINT ( 'NONE',  ( -18.05918829504999934, 10.97290950744599947, 57.35000000000000142 ) ) ;
#13587 = DIRECTION ( 'NONE',  ( -1.000000000000000000, 0.000000000000000000, 0.000000000000000000 ) ) ;
#13588 = LINE ( 'NONE', #2866, #10087 ) ;
#13589 = CARTESIAN_POINT ( 'NONE',  ( -18.05918829504999934, 10.97290950744599947, 64.35000000000000853 ) ) ;
#13590 = CARTESIAN_POINT ( 'NONE',  ( -18.05918829504999934, 10.97290950744599947, 64.35000000000000853 ) ) ;
#13591 = CARTESIAN_POINT ( 'NONE',  ( -10.81426999815532852, 15.06602133594271820, 7.000000000000000000 ) ) ;
#13592 = EDGE_CURVE ( 'NONE', #759, #10847, #10666, .T. ) ;
#13593 = LINE ( 'NONE', #2095, #12962 ) ;
#13594 = DIRECTION ( 'NONE',  ( 1.000000000000000000, 0.000000000000000000, 0.000000000000000000 ) ) ;
#13595 = DIRECTION ( 'NONE',  ( 0.7091883091770476710, -0.7050191076322684935, 0.000000000000000000 ) ) ;
#13596 = AXIS2_PLACEMENT_3D ( 'NONE', #2233, #6471, #2030 ) ;
#13597 = ORIENTED_EDGE ( 'NONE', *, *, #6358, .F. ) ;
#13598 = EDGE_LOOP ( 'NONE', ( #9372, #306 ) ) ;
#13599 = AXIS2_PLACEMENT_3D ( 'NONE', #3630, #6756, #334 ) ;
#13600 = DIRECTION ( 'NONE',  ( 0.6615960714621569316, -0.7498604124941123938, 0.000000000000000000 ) ) ;
#13601 = ORIENTED_EDGE ( 'NONE', *, *, #9657, .T. ) ;
#13602 = VECTOR ( 'NONE', #71, 1000.000000000000000 ) ;
#13603 = EDGE_CURVE ( 'NONE', #8732, #10843, #3108, .T. ) ;
#13604 = AXIS2_PLACEMENT_3D ( 'NONE', #9818, #4505, #8760 ) ;
#13605 = EDGE_LOOP ( 'NONE', ( #7034, #10675, #8503, #13764 ) ) ;
#13606 = ORIENTED_EDGE ( 'NONE', *, *, #8767, .T. ) ;
#13607 = CARTESIAN_POINT ( 'NONE',  ( -5.631644894983189431, 10.97290950744599947, 64.85000000000000853 ) ) ;
#13608 = DIRECTION ( 'NONE',  ( 0.000000000000000000, 0.000000000000000000, 1.000000000000000000 ) ) ;
#13609 = DIRECTION ( 'NONE',  ( -0.000000000000000000, 1.000000000000000000, -0.000000000000000000 ) ) ;
#13610 = ORIENTED_EDGE ( 'NONE', *, *, #1514, .F. ) ;
#13611 = DIRECTION ( 'NONE',  ( 0.000000000000000000, 0.000000000000000000, -1.000000000000000000 ) ) ;
#13612 = EDGE_CURVE ( 'NONE', #1587, #2494, #417, .T. ) ;
#13613 = DIRECTION ( 'NONE',  ( -0.000000000000000000, 0.000000000000000000, -1.000000000000000000 ) ) ;
#13614 = CARTESIAN_POINT ( 'NONE',  ( -16.04064420431702942, 4.500000000000000000, -9.307586582922249718 ) ) ;
#13615 = AXIS2_PLACEMENT_3D ( 'NONE', #3687, #9052, #3754 ) ;
#13616 = VECTOR ( 'NONE', #11234, 1000.000000000000000 ) ;
#13617 = ORIENTED_EDGE ( 'NONE', *, *, #8313, .F. ) ;
#13618 = CARTESIAN_POINT ( 'NONE',  ( -14.52722204234322945, 30.09020406744985365, 59.02705628552431705 ) ) ;
#13619 = ORIENTED_EDGE ( 'NONE', *, *, #3652, .T. ) ;
#13620 = ORIENTED_EDGE ( 'NONE', *, *, #4353, .T. ) ;
#13621 = ORIENTED_EDGE ( 'NONE', *, *, #5025, .T. ) ;
#13622 = CARTESIAN_POINT ( 'NONE',  ( -35.05918829505000645, 27.97290950744599769, 17.25000000000000000 ) ) ;
#13623 = AXIS2_PLACEMENT_3D ( 'NONE', #12444, #1904, #11532 ) ;
#13624 = DIRECTION ( 'NONE',  ( -0.000000000000000000, 1.000000000000000000, -0.000000000000000000 ) ) ;
#13625 = CARTESIAN_POINT ( 'NONE',  ( 134.8856359024541973, 103.9054980190242361, 23.00000000000000000 ) ) ;
#13626 = ORIENTED_EDGE ( 'NONE', *, *, #490, .T. ) ;
#13627 = DIRECTION ( 'NONE',  ( 0.000000000000000000, 0.000000000000000000, -1.000000000000000000 ) ) ;
#13628 = DIRECTION ( 'NONE',  ( -0.000000000000000000, -0.000000000000000000, 1.000000000000000000 ) ) ;
#13629 = EDGE_CURVE ( 'NONE', #11674, #8206, #13570, .T. ) ;
#13630 = ORIENTED_EDGE ( 'NONE', *, *, #10795, .F. ) ;
#13631 = CARTESIAN_POINT ( 'NONE',  ( -35.05918829505000645, 27.97290950744599769, 7.250000000000000000 ) ) ;
#13632 = DIRECTION ( 'NONE',  ( -0.9496839325805410681, 0.3132098788326420080, 0.000000000000000000 ) ) ;
#13633 = CARTESIAN_POINT ( 'NONE',  ( -18.05918829504999934, 10.97290950744599947, 58.54999999999999716 ) ) ;
#13634 = CYLINDRICAL_SURFACE ( 'NONE', #4013, 4.250000000000000000 ) ;
#13635 = EDGE_CURVE ( 'NONE', #13545, #3128, #7096, .T. ) ;
#13636 = CIRCLE ( 'NONE', #2056, 2.500000000000000000 ) ;
#13637 =( BOUNDED_CURVE ( )  B_SPLINE_CURVE ( 3, ( #453, #10104, #8980, #3676 ),
 .UNSPECIFIED., .F., .F. ) 
 B_SPLINE_CURVE_WITH_KNOTS ( ( 4, 4 ),
 ( 1.570796326794896558, 3.141592653589793116 ),
 .UNSPECIFIED. ) 
 CURVE ( )  GEOMETRIC_REPRESENTATION_ITEM ( )  RATIONAL_B_SPLINE_CURVE ( ( 1.000000000000000000, 0.8047378541243649375, 0.8047378541243649375, 1.000000000000000000 ) ) 
 REPRESENTATION_ITEM ( '' )  );
#13638 = EDGE_CURVE ( 'NONE', #7318, #3046, #5705, .T. ) ;
#13639 = VECTOR ( 'NONE', #3952, 1000.000000000000000 ) ;
#13640 = VERTEX_POINT ( 'NONE', #6966 ) ;
#13641 = ORIENTED_EDGE ( 'NONE', *, *, #11973, .T. ) ;
#13642 = ORIENTED_EDGE ( 'NONE', *, *, #10146, .T. ) ;
#13643 = ORIENTED_EDGE ( 'NONE', *, *, #2631, .T. ) ;
#13644 = ORIENTED_EDGE ( 'NONE', *, *, #5261, .T. ) ;
#13645 = EDGE_LOOP ( 'NONE', ( #2558, #12740, #4625, #5084 ) ) ;
#13646 = ORIENTED_EDGE ( 'NONE', *, *, #584, .F. ) ;
#13647 = CARTESIAN_POINT ( 'NONE',  ( -14.82135136386927954, 17.34777515364455169, 64.85000000000000853 ) ) ;
#13648 = EDGE_CURVE ( 'NONE', #3038, #6850, #9108, .T. ) ;
#13649 = DIRECTION ( 'NONE',  ( 0.000000000000000000, 0.000000000000000000, 1.000000000000000000 ) ) ;
#13650 = CARTESIAN_POINT ( 'NONE',  ( 10.81426999815522549, -15.06602133594279991, -3.000000000000000000 ) ) ;
#13651 = DIRECTION ( 'NONE',  ( 0.000000000000000000, -1.000000000000000000, 0.000000000000000000 ) ) ;
#13652 = DIRECTION ( 'NONE',  ( 0.000000000000000000, 0.000000000000000000, 1.000000000000000000 ) ) ;
#13653 = CARTESIAN_POINT ( 'NONE',  ( 0.000000000000000000, 0.000000000000000000, 6.000000000000000888 ) ) ;
#13654 = SHAPE_DEFINITION_REPRESENTATION ( #4411, #11399 ) ;
#13655 = ORIENTED_EDGE ( 'NONE', *, *, #3685, .F. ) ;
#13656 = ORIENTED_EDGE ( 'NONE', *, *, #12183, .T. ) ;
#13657 = ADVANCED_FACE ( 'NONE', ( #13321 ), #5642, .T. ) ;
#13658 = CIRCLE ( 'NONE', #9646, 1.999999999999996669 ) ;
#13659 = ORIENTED_EDGE ( 'NONE', *, *, #1915, .F. ) ;
#13660 = DIRECTION ( 'NONE',  ( -0.1325514707600310149, -1.623287343885459848E-17, -0.9911761234005551646 ) ) ;
#13661 = ORIENTED_EDGE ( 'NONE', *, *, #9195, .F. ) ;
#13662 = ORIENTED_EDGE ( 'NONE', *, *, #1598, .F. ) ;
#13663 = CARTESIAN_POINT ( 'NONE',  ( -43.05918829505002066, 32.97290950744599769, 10.00000000000000000 ) ) ;
#13664 = LINE ( 'NONE', #6109, #3297 ) ;
#13665 = CARTESIAN_POINT ( 'NONE',  ( -3.759188295049999518, -6.027090492554000534, 64.85000000000000853 ) ) ;
#13666 = DIRECTION ( 'NONE',  ( 1.000000000000000000, 0.000000000000000000, 0.000000000000000000 ) ) ;
#13667 = VERTEX_POINT ( 'NONE', #2741 ) ;
#13668 = LINE ( 'NONE', #5972, #12253 ) ;
#13669 = DIRECTION ( 'NONE',  ( 0.000000000000000000, 0.000000000000000000, -1.000000000000000000 ) ) ;
#13670 = FACE_BOUND ( 'NONE', #5850, .T. ) ;
#13671 = VECTOR ( 'NONE', #4581, 1000.000000000000114 ) ;
#13672 = ORIENTED_EDGE ( 'NONE', *, *, #13723, .T. ) ;
#13673 = EDGE_CURVE ( 'NONE', #3038, #8537, #410, .T. ) ;
#13674 = EDGE_CURVE ( 'NONE', #2401, #2781, #13193, .T. ) ;
#13675 = ORIENTED_EDGE ( 'NONE', *, *, #5766, .T. ) ;
#13676 = ORIENTED_EDGE ( 'NONE', *, *, #2965, .T. ) ;
#13677 = CARTESIAN_POINT ( 'NONE',  ( -18.05918829504999934, 10.97290950744599947, 24.10000000000000142 ) ) ;
#13678 = CARTESIAN_POINT ( 'NONE',  ( -20.17037093922029456, 15.77813698237436668, 68.60160116090442273 ) ) ;
#13679 = DIRECTION ( 'NONE',  ( 0.000000000000000000, 0.000000000000000000, -1.000000000000000000 ) ) ;
#13680 = CARTESIAN_POINT ( 'NONE',  ( 140.6356359024541973, 94.90549801902425031, 20.00000000000000000 ) ) ;
#13681 = CARTESIAN_POINT ( 'NONE',  ( 0.000000000000000000, 90.15549801902423610, 22.75000000000000000 ) ) ;
#13682 = AXIS2_PLACEMENT_3D ( 'NONE', #12626, #12418, #3078 ) ;
#13683 = ADVANCED_FACE ( 'NONE', ( #1521 ), #5778, .F. ) ;
#13684 = VERTEX_POINT ( 'NONE', #1663 ) ;
#13685 = EDGE_CURVE ( 'NONE', #8747, #9710, #10196, .T. ) ;
#13686 = CARTESIAN_POINT ( 'NONE',  ( -15.75919308146518283, 30.24616810854943694, 60.82807559156996291 ) ) ;
#13687 = VERTEX_POINT ( 'NONE', #8937 ) ;
#13688 = ORIENTED_EDGE ( 'NONE', *, *, #9612, .F. ) ;
#13689 = ORIENTED_EDGE ( 'NONE', *, *, #1008, .F. ) ;
#13690 = DIRECTION ( 'NONE',  ( -1.000000000000000000, 0.000000000000000000, 0.000000000000000000 ) ) ;
#13691 = LINE ( 'NONE', #11465, #2490 ) ;
#13692 = DIRECTION ( 'NONE',  ( 0.7071067811865425767, -0.7071067811865524577, 0.000000000000000000 ) ) ;
#13693 = ORIENTED_EDGE ( 'NONE', *, *, #10582, .T. ) ;
#13694 = DIRECTION ( 'NONE',  ( -1.000000000000000000, 0.000000000000000000, 0.000000000000000000 ) ) ;
#13695 = CARTESIAN_POINT ( 'NONE',  ( 140.6356359024541689, 85.03908161011133870, 20.00000000000000000 ) ) ;
#13696 = CARTESIAN_POINT ( 'NONE',  ( -28.87730642030694739, 29.81324547859995278, 5.250000000000000000 ) ) ;
#13697 = CARTESIAN_POINT ( 'NONE',  ( -16.55918829504999579, 27.90660372932210009, 57.35000000000000142 ) ) ;
#13698 = DIRECTION ( 'NONE',  ( -1.000000000000000000, -0.000000000000000000, -0.000000000000000000 ) ) ;
#13699 = ORIENTED_EDGE ( 'NONE', *, *, #13715, .F. ) ;
#13700 = ADVANCED_FACE ( 'NONE', ( #13117 ), #13394, .F. ) ;
#13701 = EDGE_CURVE ( 'NONE', #6080, #10198, #6042, .T. ) ;
#13702 = ORIENTED_EDGE ( 'NONE', *, *, #6171, .T. ) ;
#13703 = EDGE_LOOP ( 'NONE', ( #778, #10492, #12347, #4851 ) ) ;
#13704 = ORIENTED_EDGE ( 'NONE', *, *, #8316, .F. ) ;
#13705 = VERTEX_POINT ( 'NONE', #7873 ) ;
#13706 = DIRECTION ( 'NONE',  ( -0.6615960714621568206, 0.7498604124941127269, 0.000000000000000000 ) ) ;
#13707 = CARTESIAN_POINT ( 'NONE',  ( 20.45469220996244175, 1.832421873814834123, 0.000000000000000000 ) ) ;
#13708 = ORIENTED_EDGE ( 'NONE', *, *, #9080, .F. ) ;
#13709 = DIRECTION ( 'NONE',  ( -1.000000000000000000, 5.059610138265691632E-16, 0.000000000000000000 ) ) ;
#13710 = CARTESIAN_POINT ( 'NONE',  ( -18.92810326151374056, 26.94929807862704507, 56.12730036355915075 ) ) ;
#13711 = CARTESIAN_POINT ( 'NONE',  ( -18.05918829504999934, 7.130333642789880244, 64.85000000000000853 ) ) ;
#13712 = LINE ( 'NONE', #11425, #2512 ) ;
#13713 = VECTOR ( 'NONE', #9165, 1000.000000000000000 ) ;
#13714 = LINE ( 'NONE', #12809, #1334 ) ;
#13715 = EDGE_CURVE ( 'NONE', #4079, #1108, #3571, .T. ) ;
#13716 = ORIENTED_EDGE ( 'NONE', *, *, #12274, .T. ) ;
#13717 = AXIS2_PLACEMENT_3D ( 'NONE', #13403, #2875, #3022 ) ;
#13718 = CARTESIAN_POINT ( 'NONE',  ( 4.500000000000002665, -0.5000000000000005551, -65.00000000000000000 ) ) ;
#13719 = LINE ( 'NONE', #4169, #3339 ) ;
#13720 = ORIENTED_EDGE ( 'NONE', *, *, #13306, .F. ) ;
#13721 = CARTESIAN_POINT ( 'NONE',  ( -35.05918829505000645, -6.027090492554000534, 58.85000000000000142 ) ) ;
#13722 = CARTESIAN_POINT ( 'NONE',  ( -6.000000000000000888, -12.00000000000000178, 7.000000000000000000 ) ) ;
#13723 = EDGE_CURVE ( 'NONE', #11467, #1998, #12247, .T. ) ;
#13724 = CARTESIAN_POINT ( 'NONE',  ( -34.21361676484809777, 5.678153534393399759, 62.14999999999999858 ) ) ;
#13725 = CYLINDRICAL_SURFACE ( 'NONE', #2762, 0.2500000000000002220 ) ;
#13726 = CYLINDRICAL_SURFACE ( 'NONE', #10917, 17.00000000000000000 ) ;
#13727 = CARTESIAN_POINT ( 'NONE',  ( -35.05918829505000645, -6.027090492554000534, 58.85000000000000142 ) ) ;
#13728 = CARTESIAN_POINT ( 'NONE',  ( 3.500000000000001776, 2.000000000000000000, -65.00000000000000000 ) ) ;
#13729 = FACE_BOUND ( 'NONE', #8716, .T. ) ;
#13730 = PLANE ( 'NONE',  #7999 ) ;
#13731 = VECTOR ( 'NONE', #13660, 1000.000000000000114 ) ;
#13732 = ADVANCED_FACE ( 'NONE', ( #11442, #1812, #3968, #8300, #967, #6185 ), #13730, .F. ) ;
#13733 = ORIENTED_EDGE ( 'NONE', *, *, #2194, .T. ) ;
#13734 = LINE ( 'NONE', #11660, #7443 ) ;
#13735 = ORIENTED_EDGE ( 'NONE', *, *, #4324, .T. ) ;
#13736 = ORIENTED_EDGE ( 'NONE', *, *, #8592, .F. ) ;
#13737 = ORIENTED_EDGE ( 'NONE', *, *, #10201, .F. ) ;
#13738 = CARTESIAN_POINT ( 'NONE',  ( 134.6356359024541973, 108.6554980190242503, 23.00000000000000000 ) ) ;
#13739 = VECTOR ( 'NONE', #4236, 1000.000000000000114 ) ;
#13740 = EDGE_CURVE ( 'NONE', #7715, #3533, #6269, .T. ) ;
#13741 = DIRECTION ( 'NONE',  ( 1.000000000000000000, 0.000000000000000000, 0.000000000000000000 ) ) ;
#13742 = DIRECTION ( 'NONE',  ( 0.000000000000000000, 0.000000000000000000, 1.000000000000000000 ) ) ;
#13743 = CARTESIAN_POINT ( 'NONE',  ( -15.84935410452223792, 6.254721532704953901, 68.64057313984737618 ) ) ;
#13744 = FACE_OUTER_BOUND ( 'NONE', #5189, .T. ) ;
#13745 = MECHANICAL_DESIGN_GEOMETRIC_PRESENTATION_REPRESENTATION (  '', ( #812 ), #7718 ) ;
#13746 = CARTESIAN_POINT ( 'NONE',  ( -14.54431709152540897, 30.09282919894160813, 59.07233549947221718 ) ) ;
#13747 = VERTEX_POINT ( 'NONE', #5152 ) ;
#13748 = ORIENTED_EDGE ( 'NONE', *, *, #3990, .T. ) ;
#13749 = VERTEX_POINT ( 'NONE', #12488 ) ;
#13750 = PLANE ( 'NONE',  #9296 ) ;
#13751 = DIRECTION ( 'NONE',  ( -0.000000000000000000, 1.000000000000000000, -0.000000000000000000 ) ) ;
#13752 = VECTOR ( 'NONE', #98, 1000.000000000000000 ) ;
#13753 = DIRECTION ( 'NONE',  ( 0.000000000000000000, 0.000000000000000000, 1.000000000000000000 ) ) ;
#13754 = DIRECTION ( 'NONE',  ( -1.000000000000000000, 0.000000000000000000, 0.000000000000000000 ) ) ;
#13755 = CARTESIAN_POINT ( 'NONE',  ( -18.05918829504999934, 10.97290950744599947, 11.50000000000000000 ) ) ;
#13756 = CIRCLE ( 'NONE', #12658, 2.700000000000000178 ) ;
#13757 = CARTESIAN_POINT ( 'NONE',  ( -1.433900126049995061, 2.660265422446006500, 63.26601075299999621 ) ) ;
#13758 = EDGE_CURVE ( 'NONE', #11456, #12316, #8092, .T. ) ;
#13759 = CARTESIAN_POINT ( 'NONE',  ( -24.65502162805000097, 10.97290950744599947, 60.40999999999999659 ) ) ;
#13760 = AXIS2_PLACEMENT_3D ( 'NONE', #8406, #12675, #3126 ) ;
#13761 = AXIS2_PLACEMENT_3D ( 'NONE', #9482, #5072, #676 ) ;
#13762 = ORIENTED_EDGE ( 'NONE', *, *, #7416, .F. ) ;
#13763 = AXIS2_PLACEMENT_3D ( 'NONE', #2089, #4172, #7421 ) ;
#13764 = ORIENTED_EDGE ( 'NONE', *, *, #1540, .F. ) ;
#13765 = VERTEX_POINT ( 'NONE', #9278 ) ;
#13766 = EDGE_LOOP ( 'NONE', ( #12973, #5260, #7332, #10235 ) ) ;
#13767 = CARTESIAN_POINT ( 'NONE',  ( -35.05918829505000645, -6.027090492554000534, 64.85000000000000853 ) ) ;
#13768 = CARTESIAN_POINT ( 'NONE',  ( -27.49999999999998934, 9.000000000000000000, 29.99999999999999645 ) ) ;
#13769 = VERTEX_POINT ( 'NONE', #3079 ) ;
#13770 = DIRECTION ( 'NONE',  ( 0.000000000000000000, 0.000000000000000000, 1.000000000000000000 ) ) ;
#13771 = VECTOR ( 'NONE', #10552, 1000.000000000000000 ) ;
#13772 = DIRECTION ( 'NONE',  ( -1.000000000000000000, 0.000000000000000000, 0.000000000000000000 ) ) ;
#13773 = DIRECTION ( 'NONE',  ( 0.000000000000000000, 0.000000000000000000, -1.000000000000000000 ) ) ;
#13774 = CIRCLE ( 'NONE', #7512, 4.250000000000003553 ) ;
#13775 = DIRECTION ( 'NONE',  ( -0.000000000000000000, 1.000000000000000000, -0.000000000000000000 ) ) ;
#13776 = EDGE_CURVE ( 'NONE', #7296, #223, #7523, .T. ) ;
#13777 = VECTOR ( 'NONE', #11002, 1000.000000000000227 ) ;
#13778 = CARTESIAN_POINT ( 'NONE',  ( -1.059188295049996231, 27.97290950744599769, 10.00000000000000000 ) ) ;
#13779 = ITEM_DEFINED_TRANSFORMATION ( 'NONE', 'NONE', #3337,  #6434 ) ;
#13780 = CIRCLE ( 'NONE', #5978, 16.95000000000000284 ) ;
#13781 = AXIS2_PLACEMENT_3D ( 'NONE', #13304, #11986, #11922 ) ;
#13782 = ORIENTED_EDGE ( 'NONE', *, *, #3991, .T. ) ;
#13783 = CIRCLE ( 'NONE', #423, 16.50000000000000000 ) ;
#13784 = CARTESIAN_POINT ( 'NONE',  ( 76.11748380738829667, 115.4601262030644762, 0.7500000000000006661 ) ) ;
#13785 = DIRECTION ( 'NONE',  ( 0.000000000000000000, 0.000000000000000000, 1.000000000000000000 ) ) ;
#13786 = DIRECTION ( 'NONE',  ( -0.000000000000000000, -1.000000000000000000, -0.000000000000000000 ) ) ;
#13787 =( NAMED_UNIT ( * ) PLANE_ANGLE_UNIT ( ) SI_UNIT ( $, .RADIAN. ) );
#13788 = DIRECTION ( 'NONE',  ( -0.3132098788326400651, 0.9496839325805417342, 0.000000000000000000 ) ) ;
#13789 = DIRECTION ( 'NONE',  ( -0.000000000000000000, 1.000000000000000000, -0.000000000000000000 ) ) ;
#13790 = ORIENTED_EDGE ( 'NONE', *, *, #1038, .T. ) ;
#13791 = FACE_OUTER_BOUND ( 'NONE', #8595, .T. ) ;
#13792 = DIRECTION ( 'NONE',  ( -0.000000000000000000, -0.000000000000000000, -1.000000000000000000 ) ) ;
#13793 = CARTESIAN_POINT ( 'NONE',  ( -35.05918829505000645, -6.027090492554000534, 64.85000000000000853 ) ) ;
#13794 = EDGE_CURVE ( 'NONE', #9884, #13584, #5758, .T. ) ;
#13795 = DIRECTION ( 'NONE',  ( -1.000000000000000000, 1.239088197126291063E-16, -0.000000000000000000 ) ) ;
#13796 = CARTESIAN_POINT ( 'NONE',  ( -13.90184482195073912, 7.972993985840365561, 68.75388058398559110 ) ) ;
#13797 = VECTOR ( 'NONE', #7742, 1000.000000000000000 ) ;
#13798 = VECTOR ( 'NONE', #386, 1000.000000000000000 ) ;
#13799 = MANIFOLD_SOLID_BREP ( 'Fillet1', #7014 ) ;
#13800 = VECTOR ( 'NONE', #2644, 1000.000000000000000 ) ;
#13801 = EDGE_CURVE ( 'NONE', #7947, #12260, #5977, .T. ) ;
#13802 = ORIENTED_EDGE ( 'NONE', *, *, #12852, .T. ) ;
#13803 = CARTESIAN_POINT ( 'NONE',  ( -6.000000000000000888, -12.00000000000000178, 0.000000000000000000 ) ) ;
#13804 = VERTEX_POINT ( 'NONE', #10539 ) ;
#13805 = CARTESIAN_POINT ( 'NONE',  ( 42.63563590245419732, 87.03908161011136713, 19.25000000000000000 ) ) ;
#13806 = NEXT_ASSEMBLY_USAGE_OCCURRENCE ( 'NAUO1', ' ', ' ', #4332, #7890, $ ) ;
#13807 = NEXT_ASSEMBLY_USAGE_OCCURRENCE ( 'NAUO2', ' ', ' ', #4332, #11074, $ ) ;
#13808 = NEXT_ASSEMBLY_USAGE_OCCURRENCE ( 'NAUO3', ' ', ' ', #4332, #2207, $ ) ;
#13809 = NEXT_ASSEMBLY_USAGE_OCCURRENCE ( 'NAUO4', ' ', ' ', #4332, #11074, $ ) ;
#13810 = NEXT_ASSEMBLY_USAGE_OCCURRENCE ( 'NAUO5', ' ', ' ', #4332, #7890, $ ) ;
#13811 = NEXT_ASSEMBLY_USAGE_OCCURRENCE ( 'NAUO6', ' ', ' ', #4332, #10061, $ ) ;
#13812 = NEXT_ASSEMBLY_USAGE_OCCURRENCE ( 'NAUO7', ' ', ' ', #4332, #10061, $ ) ;
#13813 = NEXT_ASSEMBLY_USAGE_OCCURRENCE ( 'NAUO8', ' ', ' ', #4332, #9627, $ ) ;
#13814 = NEXT_ASSEMBLY_USAGE_OCCURRENCE ( 'NAUO9', ' ', ' ', #4332, #9627, $ ) ;
#13815 = NEXT_ASSEMBLY_USAGE_OCCURRENCE ( 'NAUO10', ' ', ' ', #4332, #566, $ ) ;
#13816 = NEXT_ASSEMBLY_USAGE_OCCURRENCE ( 'NAUO11', ' ', ' ', #4332, #738, $ ) ;
#13817 = NEXT_ASSEMBLY_USAGE_OCCURRENCE ( 'NAUO12', ' ', ' ', #4332, #12939, $ ) ;
ENDSEC;
END-ISO-10303-21;
